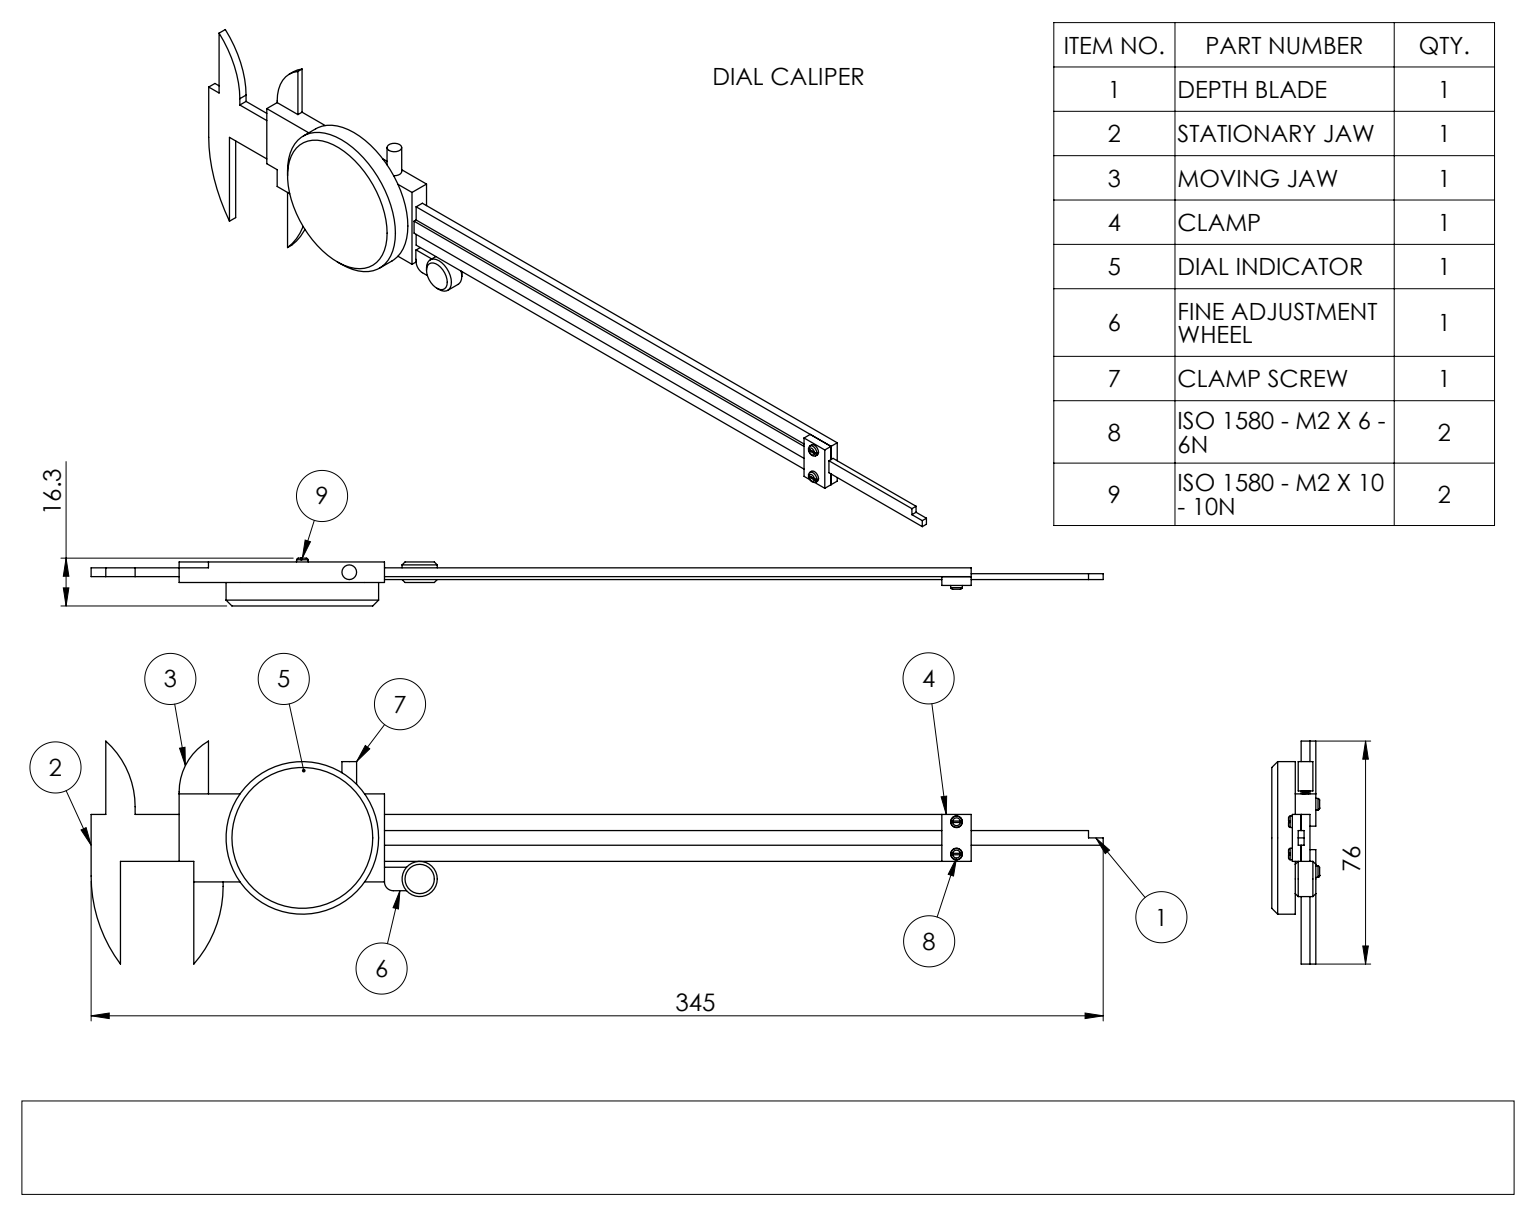
ISO-10303-21;
HEADER;
FILE_DESCRIPTION (('STEP AP214'),
    '1' );
FILE_NAME ('MAS-164',
    '2026-10-27T04:40:18',
    ( '' ),
    ( '' ),
    'SwSTEP 2.0',
    'SolidWorks 2026',
    '' );
FILE_SCHEMA (( 'AUTOMOTIVE_DESIGN' ));
ENDSEC;

DATA;
#1 = CARTESIAN_POINT ( 'NONE',  ( -49.99998799999998766, -10.00000000000001066, -0.1418111474832477736 ) ) ;
#2 = CARTESIAN_POINT ( 'NONE',  ( -60.99999999999998579, 10.72916666666666607, 2.077350269189628840 ) ) ;
#3 = CARTESIAN_POINT ( 'NONE',  ( -62.86468353124999453, 12.51562499965860198, 1.500000000000002220 ) ) ;
#4 = CARTESIAN_POINT ( 'NONE',  ( -62.43234176562498305, 9.411458332991935904, 0.7511620957034662593 ) ) ;
#5 = DIRECTION ( 'NONE',  ( 0.000000000000000000, 0.000000000000000000, -1.000000000000000000 ) ) ;
#6 = ADVANCED_FACE ( 'NONE', ( #7611 ), #3122, .F. ) ;
#7 = CARTESIAN_POINT ( 'NONE',  ( -61.99999999999998579, 16.00000000000000000, 1.500000000000002220 ) ) ;
#8 = CARTESIAN_POINT ( 'NONE',  ( -62.43234176562498305, 9.223958332991935904, 0.7511620957034662593 ) ) ;
#9 = CARTESIAN_POINT ( 'NONE',  ( 0.5000000000000000000, 0.2499999999999982792, -1.911797424705720339 ) ) ;
#10 = ORIENTED_EDGE ( 'NONE', *, *, #8889, .F. ) ;
#11 = FACE_OUTER_BOUND ( 'NONE', #2535, .T. ) ;
#12 = DIRECTION ( 'NONE',  ( -1.000000000000000000, 0.000000000000000000, 0.000000000000000000 ) ) ;
#13 = ADVANCED_FACE ( 'NONE', ( #1458 ), #5708, .T. ) ;
#14 = CARTESIAN_POINT ( 'NONE',  ( -62.86468353124998032, 15.68229166632526628, 1.000774730468978024 ) ) ;
#15 = CARTESIAN_POINT ( 'NONE',  ( -61.99999999999998579, 11.14062499965860020, 0.5015494609379544944 ) ) ;
#16 = CARTESIAN_POINT ( 'NONE',  ( -62.86468353124999453, 16.03645833299193768, 1.999225269531025750 ) ) ;
#17 = CARTESIAN_POINT ( 'NONE',  ( -61.49999999999998579, 9.677083332650534331, 2.366025403784441927 ) ) ;
#18 = ORIENTED_EDGE ( 'NONE', *, *, #1732, .F. ) ;
#19 = CARTESIAN_POINT ( 'NONE',  ( -62.49999999999998579, 14.58333333333333393, 0.6339745962155627357 ) ) ;
#20 = ADVANCED_FACE ( 'NONE', ( #3172 ), #5726, .T. ) ;
#21 = CARTESIAN_POINT ( 'NONE',  ( -61.56765823437498852, 8.598958332991934128, 2.248837904296538515 ) ) ;
#22 = SHAPE_REPRESENTATION_RELATIONSHIP ( 'NONE' , 'NONE' ,  #8867, #2558 ) ;
#23 = CARTESIAN_POINT ( 'NONE',  ( -61.49999999999998579, 13.67708333265053433, 2.366025403784441927 ) ) ;
#24 = VERTEX_POINT ( 'NONE', #10006 ) ;
#25 = DIRECTION ( 'NONE',  ( -1.000000000000000000, -0.000000000000000000, -0.000000000000000000 ) ) ;
#26 =( BOUNDED_CURVE ( )  B_SPLINE_CURVE ( 2, ( #4662, #10727, #5554, #5432, #3111, #6399, #1393, #5495, #3837 ),
 .UNSPECIFIED., .F., .T. ) 
 B_SPLINE_CURVE_WITH_KNOTS ( ( 3, 2, 2, 2, 3 ),
 ( 0.3984375000000000000, 0.4010416666666666852, 0.4062500000000000000, 0.4114583333333333148, 0.4140625000000000000 ),
 .UNSPECIFIED. ) 
 CURVE ( )  GEOMETRIC_REPRESENTATION_ITEM ( )  RATIONAL_B_SPLINE_CURVE ( ( 0.9330127018922194093, 0.9330127018922194093, 1.000000000000000000, 0.8660254037844387076, 1.000000000000000000, 0.8660254037844387076, 1.000000000000000000, 0.9330127018922194093, 0.9330127018922194093 ) ) 
 REPRESENTATION_ITEM ( '' )  );
#27 = CARTESIAN_POINT ( 'NONE',  ( -62.86468353124998032, 11.68229166632526983, 1.000774730468978024 ) ) ;
#28 = DIRECTION ( 'NONE',  ( -1.000000000000000000, 0.000000000000000000, 0.000000000000000000 ) ) ;
#29 = ORIENTED_EDGE ( 'NONE', *, *, #855, .F. ) ;
#30 = LINE ( 'NONE', #3412, #7519 ) ;
#31 = CARTESIAN_POINT ( 'NONE',  ( -62.86468353124998742, 13.28645833299193413, 1.999225269531025972 ) ) ;
#32 = CARTESIAN_POINT ( 'NONE',  ( -61.99999999999998579, 11.65624999931720218, 2.500000000000002665 ) ) ;
#33 = ORIENTED_EDGE ( 'NONE', *, *, #3045, .T. ) ;
#34 = CARTESIAN_POINT ( 'NONE',  ( -149.9999999999999716, 8.000000000000000000, 0.000000000000000000 ) ) ;
#35 = VERTEX_POINT ( 'NONE', #9289 ) ;
#36 = DIRECTION ( 'NONE',  ( 1.000000000000000000, 0.000000000000000000, 0.000000000000000000 ) ) ;
#37 = AXIS2_PLACEMENT_3D ( 'NONE', #4538, #3831, #10428 ) ;
#38 = AXIS2_PLACEMENT_3D ( 'NONE', #7635, #10225, #6696 ) ;
#39 = ADVANCED_FACE ( 'NONE', ( #10062, #3972, #586 ), #1625, .F. ) ;
#40 = VERTEX_POINT ( 'NONE', #7517 ) ;
#41 = VERTEX_POINT ( 'NONE', #5843 ) ;
#42 = CARTESIAN_POINT ( 'NONE',  ( -61.99999999999998579, 8.703124999658601979, 0.5015494609379544944 ) ) ;
#43 = CARTESIAN_POINT ( 'NONE',  ( -61.99999999999998579, 15.93749999999999645, 2.500000000000002665 ) ) ;
#44 = AXIS2_PLACEMENT_3D ( 'NONE', #893, #1059, #6847 ) ;
#45 = CARTESIAN_POINT ( 'NONE',  ( -61.13531646874998415, 12.66145833299193413, 1.000774730468978468 ) ) ;
#46 = ORIENTED_EDGE ( 'NONE', *, *, #9999, .T. ) ;
#47 = DIRECTION ( 'NONE',  ( -0.000000000000000000, -0.000000000000000000, -1.000000000000000000 ) ) ;
#48 = PRODUCT ( 'moving jaw', 'moving jaw', '', ( #5785 ) ) ;
#49 = EDGE_LOOP ( 'NONE', ( #4259, #9067, #9089, #3500, #4349, #3630, #6139, #9782 ) ) ;
#50 = AXIS2_PLACEMENT_3D ( 'NONE', #1912, #8752, #7861 ) ;
#51 = CARTESIAN_POINT ( 'NONE',  ( -62.99999999999998579, 11.57291666598387003, 0.9226497308103756012 ) ) ;
#52 = CARTESIAN_POINT ( 'NONE',  ( -62.43234176562498305, 15.66145833299193590, 0.7511620957034662593 ) ) ;
#53 = CARTESIAN_POINT ( 'NONE',  ( 144.0000000000000284, -5.500000000000000000, 3.000000000000000000 ) ) ;
#54 = CARTESIAN_POINT ( 'NONE',  ( -61.49999999999998579, 12.51041666598386826, 0.6339745962155628467 ) ) ;
#55 = CARTESIAN_POINT ( 'NONE',  ( -62.99999999999998579, 8.854166666666666075, 0.9226497308103756012 ) ) ;
#56 = CARTESIAN_POINT ( 'NONE',  ( -61.13531646874997705, 12.41145833299193413, 1.000774730468978468 ) ) ;
#57 = EDGE_CURVE ( 'NONE', #2237, #10334, #9260, .T. ) ;
#58 = CARTESIAN_POINT ( 'NONE',  ( -61.13531646874998415, 9.057291666325266277, 1.999225269531026417 ) ) ;
#59 = CARTESIAN_POINT ( 'NONE',  ( -61.49999999999998579, 9.208333333333333925, 2.366025403784441927 ) ) ;
#60 = DIRECTION ( 'NONE',  ( -1.000000000000000000, -0.000000000000000000, -0.000000000000000000 ) ) ;
#61 = CARTESIAN_POINT ( 'NONE',  ( -61.13531646874998415, 9.661458332991932352, 1.000774730468978468 ) ) ;
#62 = CARTESIAN_POINT ( 'NONE',  ( -62.99999999999998579, 14.07291666598387003, 0.9226497308103756012 ) ) ;
#63 = ORIENTED_EDGE ( 'NONE', *, *, #6322, .T. ) ;
#64 = VECTOR ( 'NONE', #9723, 1000.000000000000000 ) ;
#65 = CARTESIAN_POINT ( 'NONE',  ( -61.99999999999998579, 12.81250000000000000, 0.5000000000000013323 ) ) ;
#66 = CARTESIAN_POINT ( 'NONE',  ( -61.73205080756886076, 11.16741454900183328, 2.500000000000003109 ) ) ;
#67 = CARTESIAN_POINT ( 'NONE',  ( -61.99999999999999289, 15.14062499965860198, 0.5015494609379544944 ) ) ;
#68 = CARTESIAN_POINT ( 'NONE',  ( -62.43234176562499016, 10.74479166632526805, 2.248837904296538071 ) ) ;
#69 = CARTESIAN_POINT ( 'NONE',  ( -61.99999999999999289, 15.82812499965860198, 2.498450539062049724 ) ) ;
#70 = CARTESIAN_POINT ( 'NONE',  ( -37.99999999999999289, -14.00000000000000888, -2.000000000000000000 ) ) ;
#71 = EDGE_LOOP ( 'NONE', ( #7087, #10551, #5486, #977 ) ) ;
#72 = CARTESIAN_POINT ( 'NONE',  ( -62.49999999999998579, 15.08333333333333393, 0.6339745962155627357 ) ) ;
#73 = CARTESIAN_POINT ( 'NONE',  ( -62.86468353124999453, 8.286458332991934128, 1.999225269531025750 ) ) ;
#74 = CARTESIAN_POINT ( 'NONE',  ( -62.49999999999998579, 13.30208333265053433, 0.6339745962155627357 ) ) ;
#75 = CARTESIAN_POINT ( 'NONE',  ( -62.99999999999998579, 13.12500000000000178, 1.500000000000001998 ) ) ;
#76 = CARTESIAN_POINT ( 'NONE',  ( -61.99999999999998579, 9.812500000000000000, 0.5000000000000013323 ) ) ;
#77 = CARTESIAN_POINT ( 'NONE',  ( -61.56765823437498852, 11.03645833299193590, 2.248837904296538515 ) ) ;
#78 =( NAMED_UNIT ( * ) SI_UNIT ( $, .STERADIAN. ) SOLID_ANGLE_UNIT ( ) );
#79 = CARTESIAN_POINT ( 'NONE',  ( -61.99999999999997868, 8.312499999999998224, 0.5000000000000013323 ) ) ;
#80 = ORIENTED_EDGE ( 'NONE', *, *, #3705, .F. ) ;
#81 = CARTESIAN_POINT ( 'NONE',  ( -61.99999999999998579, 12.15624999931720041, 2.500000000000002665 ) ) ;
#82 = CARTESIAN_POINT ( 'NONE',  ( -61.13531646874998415, 13.16145833299193413, 1.000774730468978468 ) ) ;
#83 = SHAPE_REPRESENTATION_RELATIONSHIP ( 'NONE' , 'NONE' ,  #2047, #5753 ) ;
#84 = DIRECTION ( 'NONE',  ( -0.000000000000000000, -1.000000000000000000, -0.000000000000000000 ) ) ;
#85 = CARTESIAN_POINT ( 'NONE',  ( -60.99999999999998579, 8.697916665983868256, 2.077350269189628840 ) ) ;
#86 = ORIENTED_EDGE ( 'NONE', *, *, #4258, .T. ) ;
#87 =( BOUNDED_CURVE ( )  B_SPLINE_CURVE ( 2, ( #8357, #10903, #5902, #8456, #10798, #841, #3187, #174, #6119 ),
 .UNSPECIFIED., .F., .T. ) 
 B_SPLINE_CURVE_WITH_KNOTS ( ( 3, 2, 2, 2, 3 ),
 ( 0.5703125000000000000, 0.5729166666666666297, 0.5781250000000000000, 0.5833333333333333703, 0.5859375000000000000 ),
 .UNSPECIFIED. ) 
 CURVE ( )  GEOMETRIC_REPRESENTATION_ITEM ( )  RATIONAL_B_SPLINE_CURVE ( ( 0.9330127018922194093, 0.9330127018922194093, 1.000000000000000000, 0.8660254037844387076, 1.000000000000000000, 0.8660254037844387076, 1.000000000000000000, 0.9330127018922194093, 0.9330127018922194093 ) ) 
 REPRESENTATION_ITEM ( '' )  );
#88 = DIRECTION ( 'NONE',  ( -0.000000000000000000, 1.000000000000000000, 1.224646799147353207E-16 ) ) ;
#89 = ORIENTED_EDGE ( 'NONE', *, *, #6443, .F. ) ;
#90 = CARTESIAN_POINT ( 'NONE',  ( 11.30000000000000426, 1.224646799147353207E-16, -1.000000000000000000 ) ) ;
#91 = EDGE_CURVE ( 'NONE', #7478, #353, #1465, .T. ) ;
#92 = CARTESIAN_POINT ( 'NONE',  ( -62.43234176562498305, 11.91145833299193413, 0.7511620957034662593 ) ) ;
#93 = ORIENTED_EDGE ( 'NONE', *, *, #6556, .F. ) ;
#94 = CARTESIAN_POINT ( 'NONE',  ( -62.43234176562499016, 9.057291666325268054, 2.248837904296538071 ) ) ;
#95 = LINE ( 'NONE', #7549, #8153 ) ;
#96 = CARTESIAN_POINT ( 'NONE',  ( -61.56765823437498852, 12.59895833299193413, 2.248837904296538515 ) ) ;
#97 = EDGE_CURVE ( 'NONE', #8537, #7681, #4845, .T. ) ;
#98 = CARTESIAN_POINT ( 'NONE',  ( -61.99999999999998579, 8.281249999317202182, 0.5000000000000013323 ) ) ;
#99 = ORIENTED_EDGE ( 'NONE', *, *, #1134, .T. ) ;
#100 = CARTESIAN_POINT ( 'NONE',  ( -61.99999999999998579, 16.00000000000000000, 2.500000000000000444 ) ) ;
#101 = ORIENTED_EDGE ( 'NONE', *, *, #9521, .F. ) ;
#102 = CARTESIAN_POINT ( 'NONE',  ( -61.73205080756886076, 14.27008544963257108, 0.5000000000000014433 ) ) ;
#103 = CARTESIAN_POINT ( 'NONE',  ( -61.13531646874998415, 15.30729166632526983, 1.999225269531026417 ) ) ;
#104 = FACE_OUTER_BOUND ( 'NONE', #8107, .T. ) ;
#105 = CARTESIAN_POINT ( 'NONE',  ( 140.0000000000000284, 8.000000000000000000, 3.000000000000000000 ) ) ;
#106 = CARTESIAN_POINT ( 'NONE',  ( -62.49999999999998579, 12.30208333265053611, 0.6339745962155627357 ) ) ;
#107 = EDGE_CURVE ( 'NONE', #8110, #4251, #4105, .T. ) ;
#108 = CARTESIAN_POINT ( 'NONE',  ( -61.56765823437498852, 14.34895833299193413, 2.248837904296538515 ) ) ;
#109 = CARTESIAN_POINT ( 'NONE',  ( -62.43234176562499016, 8.494791666325268054, 2.248837904296538071 ) ) ;
#110 = CARTESIAN_POINT ( 'NONE',  ( -61.99999999999998579, 9.187500000000000000, 2.500000000000002665 ) ) ;
#111 = LINE ( 'NONE', #735, #8321 ) ;
#112 = CARTESIAN_POINT ( 'NONE',  ( -61.56765823437498142, 8.682291666325268054, 0.7511620957034663704 ) ) ;
#113 = ADVANCED_FACE ( 'NONE', ( #788 ), #9184, .T. ) ;
#114 = CARTESIAN_POINT ( 'NONE',  ( -62.49999999999998579, 14.05208333265053611, 0.6339745962155627357 ) ) ;
#115 = EDGE_LOOP ( 'NONE', ( #2530, #9133, #537, #4365 ) ) ;
#116 = PLANE ( 'NONE',  #5116 ) ;
#117 = DIRECTION ( 'NONE',  ( 0.000000000000000000, 0.000000000000000000, 1.000000000000000000 ) ) ;
#118 = EDGE_CURVE ( 'NONE', #7049, #4198, #6685, .T. ) ;
#119 = CARTESIAN_POINT ( 'NONE',  ( -61.13531646874998415, 15.07812499965860020, 1.500000000000002220 ) ) ;
#120 = CARTESIAN_POINT ( 'NONE',  ( -62.86468353124998032, 10.93229166632526805, 1.000774730468978246 ) ) ;
#121 = CARTESIAN_POINT ( 'NONE',  ( -61.56765823437498852, 9.536458332991934128, 2.248837904296538515 ) ) ;
#122 = ORIENTED_EDGE ( 'NONE', *, *, #10904, .T. ) ;
#123 = CARTESIAN_POINT ( 'NONE',  ( -62.99999999999998579, 15.12500000000000000, 1.500000000000001998 ) ) ;
#124 = CARTESIAN_POINT ( 'NONE',  ( -61.13531646874998415, 9.640624999658601979, 1.500000000000002220 ) ) ;
#125 = AXIS2_PLACEMENT_3D ( 'NONE', #8648, #2761, #6933 ) ;
#126 = CARTESIAN_POINT ( 'NONE',  ( 0.000000000000000000, 0.000000000000000000, 0.000000000000000000 ) ) ;
#127 = CARTESIAN_POINT ( 'NONE',  ( -61.49999999999998579, 13.76041666598387003, 0.6339745962155628467 ) ) ;
#128 = ORIENTED_EDGE ( 'NONE', *, *, #1993, .F. ) ;
#129 = CARTESIAN_POINT ( 'NONE',  ( -61.99999999999998579, 14.90624999931720218, 2.500000000000002665 ) ) ;
#130 = VECTOR ( 'NONE', #9095, 1000.000000000000000 ) ;
#131 = CARTESIAN_POINT ( 'NONE',  ( -62.86468353124999453, 11.97395833299193413, 1.999225269531025750 ) ) ;
#132 =( NAMED_UNIT ( * ) PLANE_ANGLE_UNIT ( ) SI_UNIT ( $, .RADIAN. ) );
#133 = LINE ( 'NONE', #9524, #10148 ) ;
#134 = ORIENTED_EDGE ( 'NONE', *, *, #6586, .T. ) ;
#135 = CARTESIAN_POINT ( 'NONE',  ( -105.0000000000000000, 2.500000000000000000, 4.000000000000000000 ) ) ;
#136 = CARTESIAN_POINT ( 'NONE',  ( -61.13531646874998415, 12.91145833299193590, 1.000774730468978468 ) ) ;
#137 = FILL_AREA_STYLE ('',( #1868 ) ) ;
#138 = CARTESIAN_POINT ( 'NONE',  ( -60.99999999999998579, 10.22916666666666785, 2.077350269189628840 ) ) ;
#139 = VECTOR ( 'NONE', #2970, 1000.000000000000000 ) ;
#140 = CARTESIAN_POINT ( 'NONE',  ( -62.49999999999998579, 9.302083332650536107, 0.6339745962155627357 ) ) ;
#141 = EDGE_CURVE ( 'NONE', #5618, #1714, #3939, .T. ) ;
#142 = ORIENTED_EDGE ( 'NONE', *, *, #7024, .F. ) ;
#143 = CARTESIAN_POINT ( 'NONE',  ( -61.73205080756886076, 14.05133545031537068, 0.5000000000000014433 ) ) ;
#144 = CIRCLE ( 'NONE', #2107, 1.000000000000000888 ) ;
#145 = CARTESIAN_POINT ( 'NONE',  ( -62.26794919243111082, 15.29241454900183328, 0.5000000000000013323 ) ) ;
#146 = EDGE_CURVE ( 'NONE', #6970, #9736, #4895, .T. ) ;
#147 = CARTESIAN_POINT ( 'NONE',  ( -61.13531646874998415, 11.05729166632526805, 1.999225269531026417 ) ) ;
#148 = VECTOR ( 'NONE', #1244, 1000.000000000000000 ) ;
#149 = ORIENTED_EDGE ( 'NONE', *, *, #772, .F. ) ;
#150 = VECTOR ( 'NONE', #8789, 1000.000000000000000 ) ;
#151 = CARTESIAN_POINT ( 'NONE',  ( -61.13531646874998415, 8.411458332991934128, 1.000774730468978468 ) ) ;
#152 = PLANE ( 'NONE',  #5103 ) ;
#153 = EDGE_CURVE ( 'NONE', #9355, #9315, #9914, .T. ) ;
#154 = VECTOR ( 'NONE', #5685, 1000.000000000000000 ) ;
#155 = CARTESIAN_POINT ( 'NONE',  ( -61.56765823437498852, 14.09895833299193413, 2.248837904296538515 ) ) ;
#156 = CARTESIAN_POINT ( 'NONE',  ( -62.49999999999998579, 9.302083332650536107, 0.6339745962155627357 ) ) ;
#157 = ORIENTED_EDGE ( 'NONE', *, *, #473, .F. ) ;
#158 = FACE_OUTER_BOUND ( 'NONE', #3006, .T. ) ;
#159 = ORIENTED_EDGE ( 'NONE', *, *, #10440, .T. ) ;
#160 = CARTESIAN_POINT ( 'NONE',  ( -62.49999999999998579, 10.83333333333333393, 0.6339745962155627357 ) ) ;
#161 = CARTESIAN_POINT ( 'NONE',  ( -62.99999999999998579, 8.104166666666667851, 0.9226497308103756012 ) ) ;
#162 = AXIS2_PLACEMENT_3D ( 'NONE', #9186, #3975, #9242 ) ;
#163 = CARTESIAN_POINT ( 'NONE',  ( -61.99999999999997868, 8.781249999317202182, 0.5000000000000013323 ) ) ;
#164 = DIRECTION ( 'NONE',  ( -0.000000000000000000, -1.000000000000000000, -0.000000000000000000 ) ) ;
#165 = CARTESIAN_POINT ( 'NONE',  ( -61.73205080756888208, 10.69866454968463110, 2.500000000000006661 ) ) ;
#166 = CARTESIAN_POINT ( 'NONE',  ( -61.13531646874997705, 13.41145833299193413, 1.000774730468978468 ) ) ;
#167 = CARTESIAN_POINT ( 'NONE',  ( -61.56765823437498142, 8.869791666325268054, 0.7511620957034663704 ) ) ;
#168 = LINE ( 'NONE', #6113, #341 ) ;
#169 = PLANE ( 'NONE',  #3525 ) ;
#170 = CARTESIAN_POINT ( 'NONE',  ( -62.86468353124998742, 9.786458332991934128, 1.999225269531025972 ) ) ;
#171 = CARTESIAN_POINT ( 'NONE',  ( -77.99999999999998579, 11.49999999999999645, 4.999999999999999112 ) ) ;
#172 = ORIENTED_EDGE ( 'NONE', *, *, #7897, .T. ) ;
#173 = DIRECTION ( 'NONE',  ( -0.000000000000000000, -0.000000000000000000, 1.000000000000000000 ) ) ;
#174 = CARTESIAN_POINT ( 'NONE',  ( -62.26794919243111082, 12.67633545031537068, 2.500000000000003109 ) ) ;
#175 = EDGE_CURVE ( 'NONE', #2979, #4700, #8697, .T. ) ;
#176 = PRODUCT_DEFINITION_FORMATION_WITH_SPECIFIED_SOURCE ( 'ANY', '', #2270, .NOT_KNOWN. ) ;
#177 = CARTESIAN_POINT ( 'NONE',  ( -62.43234176562499016, 14.99479166632526805, 2.248837904296538071 ) ) ;
#178 = CARTESIAN_POINT ( 'NONE',  ( -62.86468353124998742, 11.47395833299193590, 1.999225269531025972 ) ) ;
#179 = ADVANCED_BREP_SHAPE_REPRESENTATION ( '', ( #4912, #2307 ), #5679 ) ;
#180 = ADVANCED_FACE ( 'NONE', ( #9080 ), #7568, .T. ) ;
#181 = CARTESIAN_POINT ( 'NONE',  ( -61.13531646874998415, 8.578124999658601979, 1.500000000000002220 ) ) ;
#182 = CARTESIAN_POINT ( 'NONE',  ( -61.99999999999998579, 11.40624999931720218, 2.500000000000002665 ) ) ;
#183 = ORIENTED_EDGE ( 'NONE', *, *, #3221, .T. ) ;
#184 = CARTESIAN_POINT ( 'NONE',  ( -62.99999999999998579, 14.60416666666666785, 0.9226497308103756012 ) ) ;
#185 = CARTESIAN_POINT ( 'NONE',  ( -61.56765823437498852, 10.09895833299193413, 2.248837904296538515 ) ) ;
#186 = CARTESIAN_POINT ( 'NONE',  ( -62.99999999999998579, 13.59374999931720218, 1.500000000000001998 ) ) ;
#187 = CARTESIAN_POINT ( 'NONE',  ( -120.0000000000000000, -4.000000000000019540, -2.000000000000000000 ) ) ;
#188 = ORIENTED_EDGE ( 'NONE', *, *, #5061, .T. ) ;
#189 = CYLINDRICAL_SURFACE ( 'NONE', #9638, 0.9999999999999981126 ) ;
#190 = CARTESIAN_POINT ( 'NONE',  ( -62.86468353124998032, 10.93229166632526805, 1.000774730468978024 ) ) ;
#191 = CARTESIAN_POINT ( 'NONE',  ( -60.99999999999998579, 13.00000000000000178, 1.500000000000002220 ) ) ;
#192 = VERTEX_POINT ( 'NONE', #7412 ) ;
#193 = CARTESIAN_POINT ( 'NONE',  ( -62.49999999999998579, 10.58333333333333393, 0.6339745962155627357 ) ) ;
#194 = CARTESIAN_POINT ( 'NONE',  ( -61.73205080756886076, 15.91741454900183150, 2.500000000000003109 ) ) ;
#195 = CARTESIAN_POINT ( 'NONE',  ( -62.86468353124999453, 14.26562499965860020, 1.500000000000002220 ) ) ;
#196 = CARTESIAN_POINT ( 'NONE',  ( -62.49999999999998579, 13.91666666666666785, 2.366025403784441483 ) ) ;
#197 = ADVANCED_FACE ( 'NONE', ( #5899 ), #8198, .T. ) ;
#198 = CARTESIAN_POINT ( 'NONE',  ( -62.99999999999998579, 8.614583332650536107, 2.077350269189627952 ) ) ;
#199 = EDGE_LOOP ( 'NONE', ( #1282, #1739, #251, #2267 ) ) ;
#200 = AXIS2_PLACEMENT_3D ( 'NONE', #7285, #4873, #3159 ) ;
#201 = LINE ( 'NONE', #377, #2655 ) ;
#202 = CARTESIAN_POINT ( 'NONE',  ( -61.73205080756886076, 10.02008544963257464, 0.5000000000000014433 ) ) ;
#203 = CARTESIAN_POINT ( 'NONE',  ( -61.56765823437498142, 11.36979166632526805, 0.7511620957034663704 ) ) ;
#204 =( NAMED_UNIT ( * ) PLANE_ANGLE_UNIT ( ) SI_UNIT ( $, .RADIAN. ) );
#205 = ORIENTED_EDGE ( 'NONE', *, *, #5925, .T. ) ;
#206 = CLOSED_SHELL ( 'NONE', ( #8673, #5883, #7933, #4871, #589, #6929, #9618, #1051, #39, #10363, #9693, #7084, #2486, #5406 ) ) ;
#207 = CARTESIAN_POINT ( 'NONE',  ( -61.13531646874998415, 10.91145833299193590, 1.000774730468978468 ) ) ;
#208 = LINE ( 'NONE', #3594, #2451 ) ;
#209 = CARTESIAN_POINT ( 'NONE',  ( -61.13531646874998415, 14.16145833299193413, 1.000774730468978468 ) ) ;
#210 = CARTESIAN_POINT ( 'NONE',  ( -62.26794919243111082, 9.292414549001833279, 0.5000000000000013323 ) ) ;
#211 = VERTEX_POINT ( 'NONE', #6639 ) ;
#212 = AXIS2_PLACEMENT_3D ( 'NONE', #5369, #8063, #3772 ) ;
#213 = CARTESIAN_POINT ( 'NONE',  ( 0.5000000000000000000, -0.2499999999999997780, -1.911797424705720116 ) ) ;
#214 = VECTOR ( 'NONE', #3123, 1000.000000000000000 ) ;
#215 = B_SPLINE_CURVE_WITH_KNOTS ( 'NONE', 3,
 ( #10711, #8988, #7212, #4753, #3985, #5646 ),
 .UNSPECIFIED., .F., .F.,
 ( 4, 2, 4 ),
 ( 0.0005861251363949651497, 0.001008091297609326311, 0.001430057458823687363 ),
 .UNSPECIFIED. ) ;
#216 = ORIENTED_EDGE ( 'NONE', *, *, #8132, .T. ) ;
#217 = CARTESIAN_POINT ( 'NONE',  ( -61.99999999999998579, 15.03124999931720218, 0.5000000000000013323 ) ) ;
#218 = CARTESIAN_POINT ( 'NONE',  ( -61.99999999999998579, 8.437500000000000000, 2.654700538379254571 ) ) ;
#219 = CARTESIAN_POINT ( 'NONE',  ( -61.99999999999998579, 13.68749999999999822, 2.500000000000002665 ) ) ;
#220 = DIRECTION ( 'NONE',  ( -1.000000000000000000, -3.469446951953572774E-16, 0.000000000000000000 ) ) ;
#221 = DIRECTION ( 'NONE',  ( -0.000000000000000000, -1.000000000000000000, -0.000000000000000000 ) ) ;
#222 = AXIS2_PLACEMENT_3D ( 'NONE', #2692, #4339, #10352 ) ;
#223 = CARTESIAN_POINT ( 'NONE',  ( -62.86468353124998032, 14.49479166632526983, 1.000774730468978024 ) ) ;
#224 = VECTOR ( 'NONE', #3060, 999.9999999999998863 ) ;
#225 = CARTESIAN_POINT ( 'NONE',  ( -61.99999999999998579, 8.515624999658601979, 2.498450539062049724 ) ) ;
#226 = CARTESIAN_POINT ( 'NONE',  ( -62.99999999999998579, 11.32291666598387181, 0.9226497308103756012 ) ) ;
#227 = FACE_OUTER_BOUND ( 'NONE', #9637, .T. ) ;
#228 = CARTESIAN_POINT ( 'NONE',  ( -61.13531646874998415, 10.11979166632526805, 1.999225269531026417 ) ) ;
#229 = CARTESIAN_POINT ( 'NONE',  ( -61.99999999999998579, 14.03124999931720218, 0.5000000000000013323 ) ) ;
#230 = ORIENTED_EDGE ( 'NONE', *, *, #4677, .T. ) ;
#231 = DIRECTION ( 'NONE',  ( -1.000000000000000000, 0.000000000000000000, 0.000000000000000000 ) ) ;
#232 = CARTESIAN_POINT ( 'NONE',  ( -61.99999999999998579, 13.03124999931720218, 0.5000000000000013323 ) ) ;
#233 = APPLICATION_CONTEXT ( 'automotive_design' ) ;
#234 = VECTOR ( 'NONE', #2072, 1000.000000000000000 ) ;
#235 = CARTESIAN_POINT ( 'NONE',  ( -61.13531646874997705, 15.59895833299193590, 1.000774730468978468 ) ) ;
#236 = CARTESIAN_POINT ( 'NONE',  ( -61.56765823437498852, 13.03645833299193413, 2.248837904296538515 ) ) ;
#237 = CARTESIAN_POINT ( 'NONE',  ( -61.99999999999999289, 8.265624999658601979, 2.498450539062049724 ) ) ;
#238 = ORIENTED_EDGE ( 'NONE', *, *, #10620, .F. ) ;
#239 = CARTESIAN_POINT ( 'NONE',  ( -62.26794919243111082, 14.07366454968463110, 0.5000000000000013323 ) ) ;
#240 = CARTESIAN_POINT ( 'NONE',  ( -62.43234176562499016, 9.557291666325268054, 2.248837904296538071 ) ) ;
#241 = CARTESIAN_POINT ( 'NONE',  ( -61.56765823437498852, 14.78645833299193413, 2.248837904296538515 ) ) ;
#242 = AXIS2_PLACEMENT_3D ( 'NONE', #968, #2330, #9109 ) ;
#243 = CARTESIAN_POINT ( 'NONE',  ( -61.99999999999998579, 14.28124999931720396, 0.3452994616207497591 ) ) ;
#244 = LINE ( 'NONE', #5283, #6807 ) ;
#245 = ORIENTED_EDGE ( 'NONE', *, *, #9568, .F. ) ;
#246 = CARTESIAN_POINT ( 'NONE',  ( -61.73205080756886076, 9.801335450315370679, 0.5000000000000014433 ) ) ;
#247 = ADVANCED_FACE ( 'NONE', ( #10016 ), #2398, .F. ) ;
#248 = CARTESIAN_POINT ( 'NONE',  ( -61.13531646874998415, 12.07812499965860198, 1.500000000000002220 ) ) ;
#249 = CYLINDRICAL_SURFACE ( 'NONE', #10424, 0.9999999999999981126 ) ;
#250 = DIRECTION ( 'NONE',  ( 1.000000000000000000, 0.000000000000000000, 0.000000000000000000 ) ) ;
#251 = ORIENTED_EDGE ( 'NONE', *, *, #8511, .F. ) ;
#252 = CARTESIAN_POINT ( 'NONE',  ( -61.49999999999998579, 11.04166666666666607, 0.6339745962155628467 ) ) ;
#253 = CARTESIAN_POINT ( 'NONE',  ( -61.99999999999998579, 8.531249999317203958, 0.5000000000000013323 ) ) ;
#254 = CARTESIAN_POINT ( 'NONE',  ( -61.99999999999998579, 14.57812499965860198, 2.498450539062049724 ) ) ;
#255 =( BOUNDED_CURVE ( )  B_SPLINE_CURVE ( 2, ( #5430, #6282, #8897, #2058, #9721, #9666, #6225, #10606, #9607 ),
 .UNSPECIFIED., .F., .T. ) 
 B_SPLINE_CURVE_WITH_KNOTS ( ( 3, 2, 2, 2, 3 ),
 ( 0.08593750000000000000, 0.08854166666666667129, 0.09375000000000000000, 0.09895833333333332871, 0.1015625000000000833 ),
 .UNSPECIFIED. ) 
 CURVE ( )  GEOMETRIC_REPRESENTATION_ITEM ( )  RATIONAL_B_SPLINE_CURVE ( ( 0.9330127018922194093, 0.9330127018922194093, 1.000000000000000000, 0.8660254037844387076, 1.000000000000000000, 0.8660254037844387076, 1.000000000000000000, 0.9330127018922171889, 0.9330127018922194093 ) ) 
 REPRESENTATION_ITEM ( '' )  );
#256 =( NAMED_UNIT ( * ) SI_UNIT ( $, .STERADIAN. ) SOLID_ANGLE_UNIT ( ) );
#257 = CARTESIAN_POINT ( 'NONE',  ( -61.99999999999998579, 13.93749999999999822, 2.500000000000002665 ) ) ;
#258 = CARTESIAN_POINT ( 'NONE',  ( -62.99999999999998579, 9.364583332650536107, 2.077350269189627952 ) ) ;
#259 = ORIENTED_EDGE ( 'NONE', *, *, #9835, .T. ) ;
#260 = CARTESIAN_POINT ( 'NONE',  ( -61.49999999999998579, 13.54166666666666785, 0.6339745962155628467 ) ) ;
#261 = CARTESIAN_POINT ( 'NONE',  ( -62.49999999999998579, 15.38541666598387003, 2.366025403784441483 ) ) ;
#262 = CARTESIAN_POINT ( 'NONE',  ( -62.43234176562499016, 10.74479166632526805, 2.248837904296538071 ) ) ;
#263 = ADVANCED_FACE ( 'NONE', ( #7011 ), #2615, .T. ) ;
#264 = ORIENTED_EDGE ( 'NONE', *, *, #1352, .F. ) ;
#265 = CARTESIAN_POINT ( 'NONE',  ( -62.43234176562499016, 10.05729166632526805, 2.248837904296538071 ) ) ;
#266 = DIRECTION ( 'NONE',  ( -0.000000000000000000, -0.000000000000000000, -1.000000000000000000 ) ) ;
#267 = CARTESIAN_POINT ( 'NONE',  ( -61.13531646874998415, 13.86979166632526805, 1.999225269531026417 ) ) ;
#268 = DIRECTION ( 'NONE',  ( -1.000000000000000000, 0.000000000000000000, 0.000000000000000000 ) ) ;
#269 = ORIENTED_EDGE ( 'NONE', *, *, #9235, .F. ) ;
#270 = CARTESIAN_POINT ( 'NONE',  ( 0.000000000000000000, -0.2499999999999998335, -1.312875263449798879 ) ) ;
#271 = ORIENTED_EDGE ( 'NONE', *, *, #9771, .F. ) ;
#272 = DIRECTION ( 'NONE',  ( 0.000000000000000000, 0.000000000000000000, -1.000000000000000000 ) ) ;
#273 = CARTESIAN_POINT ( 'NONE',  ( -62.49999999999998579, 8.416666666666666075, 2.366025403784441483 ) ) ;
#274 = LINE ( 'NONE', #989, #4138 ) ;
#275 = DIRECTION ( 'NONE',  ( -0.000000000000000000, -1.000000000000000000, -0.000000000000000000 ) ) ;
#276 = DIRECTION ( 'NONE',  ( 1.000000000000000000, 0.000000000000000000, 0.000000000000000000 ) ) ;
#277 = CARTESIAN_POINT ( 'NONE',  ( -61.56765823437498142, 13.93229166632526805, 0.7511620957034663704 ) ) ;
#278 = CARTESIAN_POINT ( 'NONE',  ( -62.86468353124998742, 9.723958332991934128, 1.999225269531025972 ) ) ;
#279 = CARTESIAN_POINT ( 'NONE',  ( 0.3609765494018739029, 0.2499999999999997780, 1.888098105530058968 ) ) ;
#280 = CARTESIAN_POINT ( 'NONE',  ( -61.13531646874998415, 9.911458332991935904, 1.000774730468978468 ) ) ;
#281 = CARTESIAN_POINT ( 'NONE',  ( -62.49999999999998579, 12.08333333333333393, 0.6339745962155627357 ) ) ;
#282 = ORIENTED_EDGE ( 'NONE', *, *, #3450, .T. ) ;
#283 = EDGE_CURVE ( 'NONE', #10857, #3037, #6901, .T. ) ;
#284 = VECTOR ( 'NONE', #526, 1000.000000000000000 ) ;
#285 = FACE_BOUND ( 'NONE', #5927, .T. ) ;
#286 = CARTESIAN_POINT ( 'NONE',  ( -60.99999999999998579, 12.98958333265053611, 0.9226497308103762673 ) ) ;
#287 = ADVANCED_FACE ( 'NONE', ( #6844 ), #3445, .T. ) ;
#288 = CARTESIAN_POINT ( 'NONE',  ( -62.26794919243111082, 10.04241454900183328, 0.5000000000000013323 ) ) ;
#289 = CARTESIAN_POINT ( 'NONE',  ( -61.99999999999998579, 12.14062499965860198, 0.5015494609379544944 ) ) ;
#290 = CARTESIAN_POINT ( 'NONE',  ( -61.99999999999999289, 8.890624999658601979, 0.5015494609379544944 ) ) ;
#291 = CARTESIAN_POINT ( 'NONE',  ( -49.99999999999998579, -14.00000000000001243, 0.000000000000000000 ) ) ;
#292 = VERTEX_POINT ( 'NONE', #997 ) ;
#293 = CARTESIAN_POINT ( 'NONE',  ( -60.99999999999998579, 15.97916666666666607, 2.077350269189628840 ) ) ;
#294 = CARTESIAN_POINT ( 'NONE',  ( -61.13531646874997705, 10.41145833299193413, 1.000774730468978468 ) ) ;
#295 = DIRECTION ( 'NONE',  ( 1.000000000000000000, 0.000000000000000000, 0.000000000000000000 ) ) ;
#296 = CARTESIAN_POINT ( 'NONE',  ( -61.56765823437498142, 15.61979166632526628, 0.7511620957034663704 ) ) ;
#297 = ADVANCED_FACE ( 'NONE', ( #7844 ), #6003, .T. ) ;
#298 = CARTESIAN_POINT ( 'NONE',  ( -60.99999999999998579, 14.48958333265053788, 0.9226497308103762673 ) ) ;
#299 = FACE_BOUND ( 'NONE', #9767, .T. ) ;
#300 = ORIENTED_EDGE ( 'NONE', *, *, #8132, .F. ) ;
#301 = CYLINDRICAL_SURFACE ( 'NONE', #3236, 0.9999999999999981126 ) ;
#302 = VERTEX_POINT ( 'NONE', #9 ) ;
#303 = CARTESIAN_POINT ( 'NONE',  ( -61.56765823437498852, 12.78645833299193413, 2.248837904296538515 ) ) ;
#304 = CARTESIAN_POINT ( 'NONE',  ( -61.56765823437498142, 8.619791666325268054, 0.7511620957034663704 ) ) ;
#305 = CARTESIAN_POINT ( 'NONE',  ( -61.49999999999998579, 15.54166666666666607, 0.6339745962155628467 ) ) ;
#306 = ORIENTED_EDGE ( 'NONE', *, *, #5403, .T. ) ;
#307 = CARTESIAN_POINT ( 'NONE',  ( -61.99999999999998579, 12.18750000000000000, 2.654700538379254571 ) ) ;
#308 = LINE ( 'NONE', #2873, #10328 ) ;
#309 = CARTESIAN_POINT ( 'NONE',  ( -62.86468353124998032, 13.99479166632526983, 1.000774730468978246 ) ) ;
#310 = PLANE ( 'NONE',  #5287 ) ;
#311 = CARTESIAN_POINT ( 'NONE',  ( -61.49999999999998579, 10.26041666598387003, 0.6339745962155628467 ) ) ;
#312 = VERTEX_POINT ( 'NONE', #9336 ) ;
#313 = CARTESIAN_POINT ( 'NONE',  ( -105.0000000000000000, -2.500000000000000000, 4.000000000000000000 ) ) ;
#314 = CARTESIAN_POINT ( 'NONE',  ( -60.99999999999998579, 9.989583332650536107, 0.9226497308103762673 ) ) ;
#315 = CARTESIAN_POINT ( 'NONE',  ( -61.99999999999998579, 12.89062499965860376, 0.5015494609379544944 ) ) ;
#316 = ADVANCED_FACE ( 'NONE', ( #9447 ), #3389, .T. ) ;
#317 = CARTESIAN_POINT ( 'NONE',  ( -61.49999999999998579, 15.95833333333333215, 2.366025403784441927 ) ) ;
#318 =( BOUNDED_CURVE ( )  B_SPLINE_CURVE ( 2, ( #338, #1054, #8015, #9617, #7841, #6343, #2731, #6291, #1116 ),
 .UNSPECIFIED., .F., .T. ) 
 B_SPLINE_CURVE_WITH_KNOTS ( ( 3, 2, 2, 2, 3 ),
 ( 0.1953124999999999722, 0.1979166666666666574, 0.2031250000000000000, 0.2083333333333333426, 0.2109375000000000000 ),
 .UNSPECIFIED. ) 
 CURVE ( )  GEOMETRIC_REPRESENTATION_ITEM ( )  RATIONAL_B_SPLINE_CURVE ( ( 0.9330127018922194093, 0.9330127018922186322, 1.000000000000000000, 0.8660254037844387076, 1.000000000000000000, 0.8660254037844387076, 1.000000000000000000, 0.9330127018922194093, 0.9330127018922194093 ) ) 
 REPRESENTATION_ITEM ( '' )  );
#319 = EDGE_LOOP ( 'NONE', ( #4285, #2336, #2477, #10429 ) ) ;
#320 = EDGE_CURVE ( 'NONE', #4602, #5526, #6439, .T. ) ;
#321 = CARTESIAN_POINT ( 'NONE',  ( -61.99999999999998579, 10.20312499965860198, 0.5015494609379544944 ) ) ;
#322 = CARTESIAN_POINT ( 'NONE',  ( 0.000000000000000000, 0.000000000000000000, 0.000000000000000000 ) ) ;
#323 = CARTESIAN_POINT ( 'NONE',  ( -61.56765823437498852, 14.34895833299193413, 2.248837904296538515 ) ) ;
#324 = DIRECTION ( 'NONE',  ( 1.000000000000000000, 2.478176394252581387E-17, 0.000000000000000000 ) ) ;
#325 = EDGE_LOOP ( 'NONE', ( #10518, #10319, #10166, #3050 ) ) ;
#326 = CARTESIAN_POINT ( 'NONE',  ( 195.0000000000000000, -2.500000000000000000, 2.000000000000000000 ) ) ;
#327 = AXIS2_PLACEMENT_3D ( 'NONE', #3024, #4508, #7911 ) ;
#328 = CIRCLE ( 'NONE', #5652, 1.000000000000000888 ) ;
#329 = ORIENTED_EDGE ( 'NONE', *, *, #3272, .T. ) ;
#330 = CARTESIAN_POINT ( 'NONE',  ( -49.99998799999998766, -10.00000000000001066, 5.282956808509874826E-15 ) ) ;
#331 = CARTESIAN_POINT ( 'NONE',  ( -60.99999999999998579, 8.000000000000000000, 1.500000000000002220 ) ) ;
#332 = LINE ( 'NONE', #9669, #6281 ) ;
#333 = DIRECTION ( 'NONE',  ( 0.9961946980917455452, 0.000000000000000000, -0.08715574274765848506 ) ) ;
#334 = DIRECTION ( 'NONE',  ( 1.000000000000000000, 0.000000000000000000, 0.000000000000000000 ) ) ;
#335 = CARTESIAN_POINT ( 'NONE',  ( -62.86468353124999453, 14.26562499965860020, 1.500000000000002220 ) ) ;
#336 = CARTESIAN_POINT ( 'NONE',  ( -61.13531646874998415, 10.32812499965860198, 1.500000000000002220 ) ) ;
#337 = CARTESIAN_POINT ( 'NONE',  ( -61.99999999999998579, 13.28124999931720041, 0.5000000000000013323 ) ) ;
#338 = CARTESIAN_POINT ( 'NONE',  ( -61.99999999999998579, 9.562500000000000000, 0.5000000000000013323 ) ) ;
#339 = EDGE_CURVE ( 'NONE', #1405, #2680, #6609, .T. ) ;
#340 = CARTESIAN_POINT ( 'NONE',  ( -62.86468353124998742, 10.78645833299193413, 1.999225269531025972 ) ) ;
#341 = VECTOR ( 'NONE', #8505, 1000.000000000000000 ) ;
#342 = DIRECTION ( 'NONE',  ( 0.000000000000000000, 0.000000000000000000, 1.000000000000000000 ) ) ;
#343 = ORIENTED_EDGE ( 'NONE', *, *, #5169, .T. ) ;
#344 = CARTESIAN_POINT ( 'NONE',  ( 0.3612935698783895644, -0.2499999999999997224, -1.888152147991466023 ) ) ;
#345 = CARTESIAN_POINT ( 'NONE',  ( 0.6000000000000000888, 0.000000000000000000, 1.336466033005844434 ) ) ;
#346 = AXIS2_PLACEMENT_3D ( 'NONE', #4920, #5760, #10085 ) ;
#347 = ORIENTED_EDGE ( 'NONE', *, *, #4046, .F. ) ;
#348 = CARTESIAN_POINT ( 'NONE',  ( -61.13531646874998415, 8.140624999658601979, 1.500000000000002220 ) ) ;
#349 = CARTESIAN_POINT ( 'NONE',  ( -61.13531646874998415, 12.55729166632526805, 1.999225269531026417 ) ) ;
#350 = CARTESIAN_POINT ( 'NONE',  ( -61.56765823437498852, 8.786458332991934128, 2.248837904296538515 ) ) ;
#351 =( GEOMETRIC_REPRESENTATION_CONTEXT ( 3 ) GLOBAL_UNCERTAINTY_ASSIGNED_CONTEXT ( ( #4611 ) ) GLOBAL_UNIT_ASSIGNED_CONTEXT ( ( #2122, #3664, #4613 ) ) REPRESENTATION_CONTEXT ( 'NONE', 'WORKASPACE' ) );
#352 = FILL_AREA_STYLE_COLOUR ( '', #7255 ) ;
#353 = VERTEX_POINT ( 'NONE', #8565 ) ;
#354 = DIRECTION ( 'NONE',  ( -0.000000000000000000, -1.000000000000000000, -0.000000000000000000 ) ) ;
#355 = CARTESIAN_POINT ( 'NONE',  ( -61.99999999999999289, 10.32812499965860198, 2.498450539062049724 ) ) ;
#356 = CARTESIAN_POINT ( 'NONE',  ( 145.0000000000000284, -5.499999999999998224, 7.300000000000007816 ) ) ;
#357 = CARTESIAN_POINT ( 'NONE',  ( -62.43234176562499016, 14.74479166632526805, 2.248837904296538071 ) ) ;
#358 = VECTOR ( 'NONE', #7829, 1000.000000000000000 ) ;
#359 = CARTESIAN_POINT ( 'NONE',  ( -60.99999999999998579, 13.94791666598387003, 2.077350269189628840 ) ) ;
#360 = CYLINDRICAL_SURFACE ( 'NONE', #3974, 0.9999999999999981126 ) ;
#361 = ORIENTED_EDGE ( 'NONE', *, *, #10949, .T. ) ;
#362 = EDGE_CURVE ( 'NONE', #4689, #5869, #2786, .T. ) ;
#363 = CARTESIAN_POINT ( 'NONE',  ( -61.99999999999998579, 16.00000000000000000, 1.500000000000002220 ) ) ;
#364 = EDGE_LOOP ( 'NONE', ( #89, #5630 ) ) ;
#365 = STYLED_ITEM ( 'NONE', ( #4697 ), #179 ) ;
#366 = CARTESIAN_POINT ( 'NONE',  ( -61.13531646874998415, 12.57812499965860198, 1.500000000000002220 ) ) ;
#367 = EDGE_CURVE ( 'NONE', #1845, #302, #9832, .T. ) ;
#368 = CARTESIAN_POINT ( 'NONE',  ( -62.43234176562499016, 8.994791666325268054, 2.248837904296538071 ) ) ;
#369 = CARTESIAN_POINT ( 'NONE',  ( -62.99999999999998579, 10.59374999931720396, 1.500000000000001998 ) ) ;
#370 = EDGE_LOOP ( 'NONE', ( #10927, #3084, #707, #1709 ) ) ;
#371 = CARTESIAN_POINT ( 'NONE',  ( -62.99999999999998579, 12.87500000000000178, 1.500000000000001998 ) ) ;
#372 = DIRECTION ( 'NONE',  ( -1.000000000000000000, 0.000000000000000000, 0.000000000000000000 ) ) ;
#373 = CARTESIAN_POINT ( 'NONE',  ( -61.13531646874998415, 14.64062499965860020, 1.500000000000002220 ) ) ;
#374 = CARTESIAN_POINT ( 'NONE',  ( -62.26794919243111082, 13.92633545031537068, 2.500000000000003109 ) ) ;
#375 = CARTESIAN_POINT ( 'NONE',  ( -61.49999999999998579, 11.26041666598387003, 0.6339745962155628467 ) ) ;
#376 = ORIENTED_EDGE ( 'NONE', *, *, #2316, .F. ) ;
#377 = CARTESIAN_POINT ( 'NONE',  ( -114.9999999999999289, -7.999999999999998224, -2.000000000000000000 ) ) ;
#378 = CYLINDRICAL_SURFACE ( 'NONE', #125, 1.000000000000000888 ) ;
#379 = CARTESIAN_POINT ( 'NONE',  ( -61.13531646874998415, 12.30729166632526628, 1.999225269531026417 ) ) ;
#380 = LINE ( 'NONE', #7160, #836 ) ;
#381 = VERTEX_POINT ( 'NONE', #7734 ) ;
#382 = CARTESIAN_POINT ( 'NONE',  ( -61.13531646874998415, 10.14062499965860198, 1.500000000000002220 ) ) ;
#383 = CYLINDRICAL_SURFACE ( 'NONE', #5279, 0.9999999999999981126 ) ;
#384 = CARTESIAN_POINT ( 'NONE',  ( -62.86468353124999453, 14.76562499965860020, 1.500000000000002220 ) ) ;
#385 = DIRECTION ( 'NONE',  ( -0.000000000000000000, -1.000000000000000000, -0.000000000000000000 ) ) ;
#386 = VERTEX_POINT ( 'NONE', #1056 ) ;
#387 = CARTESIAN_POINT ( 'NONE',  ( 1.299999999999999156, 0.000000000000000000, 0.000000000000000000 ) ) ;
#388 = EDGE_CURVE ( 'NONE', #8021, #5388, #10231, .T. ) ;
#389 =( BOUNDED_CURVE ( )  B_SPLINE_CURVE ( 2, ( #8655, #9486, #5983, #9430, #1883, #5039, #9376, #1038, #1666 ),
 .UNSPECIFIED., .F., .F. ) 
 B_SPLINE_CURVE_WITH_KNOTS ( ( 3, 2, 2, 2, 3 ),
 ( 0.6484375000000000000, 0.6510416666666666297, 0.6562500000000000000, 0.6614583333333333703, 0.6640625000000000000 ),
 .UNSPECIFIED. ) 
 CURVE ( )  GEOMETRIC_REPRESENTATION_ITEM ( )  RATIONAL_B_SPLINE_CURVE ( ( 0.9330127018922194093, 0.9330127018922194093, 1.000000000000000000, 0.8660254037844387076, 1.000000000000000000, 0.8660254037844387076, 1.000000000000000000, 0.9330127018922194093, 0.9330127018922194093 ) ) 
 REPRESENTATION_ITEM ( '' )  );
#390 = AXIS2_PLACEMENT_3D ( 'NONE', #8453, #10271, #7624 ) ;
#391 = ORIENTED_EDGE ( 'NONE', *, *, #9319, .T. ) ;
#392 = DIRECTION ( 'NONE',  ( 0.000000000000000000, 5.282956808509869699E-16, 1.000000000000000000 ) ) ;
#393 = CARTESIAN_POINT ( 'NONE',  ( -60.99999999999998579, 8.479166666666666075, 2.077350269189628840 ) ) ;
#394 = CARTESIAN_POINT ( 'NONE',  ( -62.26794919243111082, 9.645085449632574637, 2.500000000000006217 ) ) ;
#395 = CARTESIAN_POINT ( 'NONE',  ( -61.99999999999998579, 14.28124999931720218, 0.5000000000000013323 ) ) ;
#396 = DIRECTION ( 'NONE',  ( -1.000000000000000000, -0.000000000000000000, -0.000000000000000000 ) ) ;
#397 = CARTESIAN_POINT ( 'NONE',  ( -62.86468353124999453, 14.78645833299193058, 1.999225269531025750 ) ) ;
#398 = CARTESIAN_POINT ( 'NONE',  ( -62.43234176562498305, 10.16145833299193413, 0.7511620957034662593 ) ) ;
#399 = PRODUCT_DEFINITION_CONTEXT ( 'detailed design', #1660, 'design' ) ;
#400 = CARTESIAN_POINT ( 'NONE',  ( -62.99999999999998579, 11.36458333265053611, 2.077350269189627952 ) ) ;
#401 = DIRECTION ( 'NONE',  ( -1.000000000000000000, 0.000000000000000000, 0.000000000000000000 ) ) ;
#402 = CIRCLE ( 'NONE', #212, 1.099999999999989875 ) ;
#403 = CARTESIAN_POINT ( 'NONE',  ( -61.13531646874998415, 11.14062499965860020, 1.500000000000002220 ) ) ;
#404 = DIRECTION ( 'NONE',  ( 0.000000000000000000, 0.000000000000000000, 1.000000000000000000 ) ) ;
#405 = ORIENTED_EDGE ( 'NONE', *, *, #8852, .F. ) ;
#406 = DIRECTION ( 'NONE',  ( 1.734723475976807094E-15, -1.000000000000000000, 0.000000000000000000 ) ) ;
#407 = UNCERTAINTY_MEASURE_WITH_UNIT (LENGTH_MEASURE( 1.000000000000000082E-05 ), #5246, 'distance_accuracy_value', 'NONE');
#408 = FACE_OUTER_BOUND ( 'NONE', #9322, .T. ) ;
#409 = EDGE_LOOP ( 'NONE', ( #9606, #6475, #9228, #1255, #10309, #5081, #6466, #4394, #2415, #6355, #391, #7202, #777, #5042 ) ) ;
#410 = VECTOR ( 'NONE', #7808, 1000.000000000000000 ) ;
#411 = CARTESIAN_POINT ( 'NONE',  ( -61.73205080756886787, 10.16741454900183150, 2.500000000000004885 ) ) ;
#412 = EDGE_CURVE ( 'NONE', #7538, #2208, #10852, .T. ) ;
#413 = CARTESIAN_POINT ( 'NONE',  ( -61.13531646874998415, 12.84895833299193413, 1.000774730468978468 ) ) ;
#414 = VECTOR ( 'NONE', #2699, 1000.000000000000000 ) ;
#415 = CARTESIAN_POINT ( 'NONE',  ( -61.56765823437498142, 10.61979166632526805, 0.7511620957034663704 ) ) ;
#416 = CARTESIAN_POINT ( 'NONE',  ( -61.99999999999998579, 16.00000000000000000, 0.5000000000000041078 ) ) ;
#417 = ORIENTED_EDGE ( 'NONE', *, *, #855, .T. ) ;
#418 = CARTESIAN_POINT ( 'NONE',  ( -60.99999999999998579, 8.468749999317202182, 1.500000000000002220 ) ) ;
#419 = CARTESIAN_POINT ( 'NONE',  ( -61.13531646874998415, 11.14062499965860020, 1.500000000000002220 ) ) ;
#420 = DIRECTION ( 'NONE',  ( 1.000000000000000000, 0.000000000000000000, 0.000000000000000000 ) ) ;
#421 = CARTESIAN_POINT ( 'NONE',  ( -61.99999999999998579, 14.76562499965859843, 2.498450539062049724 ) ) ;
#422 = CARTESIAN_POINT ( 'NONE',  ( -60.99999999999998579, 15.19791666598387181, 2.077350269189628840 ) ) ;
#423 = DIRECTION ( 'NONE',  ( 1.000000000000000000, 0.000000000000000000, 0.000000000000000000 ) ) ;
#424 = VERTEX_POINT ( 'NONE', #4552 ) ;
#425 = AXIS2_PLACEMENT_3D ( 'NONE', #5057, #4070, #1572 ) ;
#426 = DIRECTION ( 'NONE',  ( 0.000000000000000000, -0.000000000000000000, -1.000000000000000000 ) ) ;
#427 = VERTEX_POINT ( 'NONE', #7181 ) ;
#428 = CARTESIAN_POINT ( 'NONE',  ( -61.56765823437498852, 13.28645833299193413, 2.248837904296538515 ) ) ;
#429 = DIRECTION ( 'NONE',  ( -0.000000000000000000, -1.000000000000000000, -0.000000000000000000 ) ) ;
#430 = CARTESIAN_POINT ( 'NONE',  ( -104.9999999999999289, -16.54248688935409106, -2.000000000000000000 ) ) ;
#431 = ORIENTED_EDGE ( 'NONE', *, *, #7584, .F. ) ;
#432 = CARTESIAN_POINT ( 'NONE',  ( -60.99999999999998579, 12.50000000000000000, 1.500000000000002220 ) ) ;
#433 = AXIS2_PLACEMENT_3D ( 'NONE', #10103, #729, #1616 ) ;
#434 = CARTESIAN_POINT ( 'NONE',  ( -60.99999999999998579, 15.94791666598386826, 2.077350269189628840 ) ) ;
#435 = SURFACE_STYLE_USAGE ( .BOTH. , #2987 ) ;
#436 = CARTESIAN_POINT ( 'NONE',  ( -62.99999999999998579, 14.36458333265053611, 2.077350269189627952 ) ) ;
#437 = CARTESIAN_POINT ( 'NONE',  ( -62.99999999999998579, 10.86458333265053611, 2.077350269189627952 ) ) ;
#438 = ORIENTED_EDGE ( 'NONE', *, *, #7786, .T. ) ;
#439 = CARTESIAN_POINT ( 'NONE',  ( -61.99999999999998579, 8.000000000000000000, 1.500000000000002220 ) ) ;
#440 = CARTESIAN_POINT ( 'NONE',  ( -62.86468353124999453, 12.95312499965860198, 1.500000000000002220 ) ) ;
#441 = FILL_AREA_STYLE ('',( #3766 ) ) ;
#442 = ORIENTED_EDGE ( 'NONE', *, *, #9663, .T. ) ;
#443 = CARTESIAN_POINT ( 'NONE',  ( -61.56765823437498142, 10.68229166632526805, 0.7511620957034663704 ) ) ;
#444 = CARTESIAN_POINT ( 'NONE',  ( -62.26794919243111082, 12.54241454900183150, 0.5000000000000013323 ) ) ;
#445 = EDGE_CURVE ( 'NONE', #6076, #9310, #10674, .T. ) ;
#446 = CARTESIAN_POINT ( 'NONE',  ( -62.43234176562498305, 15.47395833299193590, 0.7511620957034662593 ) ) ;
#447 = CARTESIAN_POINT ( 'NONE',  ( -61.73205080756885366, 9.020085449632572860, 0.5000000000000028866 ) ) ;
#448 = ORIENTED_EDGE ( 'NONE', *, *, #4377, .F. ) ;
#449 = DIRECTION ( 'NONE',  ( 0.000000000000000000, 0.000000000000000000, 1.000000000000000000 ) ) ;
#450 = ORIENTED_EDGE ( 'NONE', *, *, #772, .T. ) ;
#451 = CARTESIAN_POINT ( 'NONE',  ( -49.99999999999998579, -8.000000000000000000, 0.000000000000000000 ) ) ;
#452 = CARTESIAN_POINT ( 'NONE',  ( -62.49999999999998579, 9.416666666666666075, 2.366025403784441483 ) ) ;
#453 = DIRECTION ( 'NONE',  ( -1.000000000000000000, 0.000000000000000000, -0.000000000000000000 ) ) ;
#454 = DIRECTION ( 'NONE',  ( 1.000000000000000000, 0.000000000000000000, 0.000000000000000000 ) ) ;
#455 = CARTESIAN_POINT ( 'NONE',  ( -61.99999999999998579, 8.937500000000001776, 2.500000000000002665 ) ) ;
#456 = CARTESIAN_POINT ( 'NONE',  ( -61.56765823437498142, 9.869791666325268054, 0.7511620957034663704 ) ) ;
#457 = CARTESIAN_POINT ( 'NONE',  ( -49.99999999999998579, -2.500000000000000444, 83.15773105863907233 ) ) ;
#458 = CARTESIAN_POINT ( 'NONE',  ( -62.49999999999998579, 8.302083332650536107, 0.6339745962155627357 ) ) ;
#459 = CARTESIAN_POINT ( 'NONE',  ( -62.86468353124998032, 10.49479166632526983, 1.000774730468978246 ) ) ;
#460 = DIRECTION ( 'NONE',  ( -1.000000000000000000, 0.000000000000000000, 0.000000000000000000 ) ) ;
#461 = EDGE_LOOP ( 'NONE', ( #7760, #1425, #10364, #3402 ) ) ;
#462 = CARTESIAN_POINT ( 'NONE',  ( -105.0000000000000000, 2.500000000000000000, 3.000000000000000000 ) ) ;
#463 = CARTESIAN_POINT ( 'NONE',  ( -62.26794919243111082, 9.073664549684631098, 0.5000000000000013323 ) ) ;
#464 = EDGE_LOOP ( 'NONE', ( #3656, #644 ) ) ;
#465 = CARTESIAN_POINT ( 'NONE',  ( 7.300000000000000711, 0.000000000000000000, 0.000000000000000000 ) ) ;
#466 = EDGE_CURVE ( 'NONE', #3158, #5222, #8079, .T. ) ;
#467 = CARTESIAN_POINT ( 'NONE',  ( -61.13531646874998415, 12.05729166632526628, 1.999225269531026417 ) ) ;
#468 = CARTESIAN_POINT ( 'NONE',  ( -62.86468353124999453, 10.20312499965860198, 1.500000000000002220 ) ) ;
#469 = DIRECTION ( 'NONE',  ( 1.000000000000000000, 0.000000000000000000, 0.000000000000000000 ) ) ;
#470 = VERTEX_POINT ( 'NONE', #8792 ) ;
#471 = CARTESIAN_POINT ( 'NONE',  ( -62.49999999999998579, 10.88541666598386826, 2.366025403784441483 ) ) ;
#472 = CARTESIAN_POINT ( 'NONE',  ( -62.86468353124999453, 11.28645833299193590, 1.999225269531025750 ) ) ;
#473 = EDGE_CURVE ( 'NONE', #4413, #2594, #6911, .T. ) ;
#474 = SHAPE_DEFINITION_REPRESENTATION ( #8222, #2752 ) ;
#475 = CARTESIAN_POINT ( 'NONE',  ( -62.43234176562499016, 15.99479166632526628, 2.248837904296538071 ) ) ;
#476 = CARTESIAN_POINT ( 'NONE',  ( -60.99999999999998579, 14.21874999931720218, 1.500000000000002220 ) ) ;
#477 = CARTESIAN_POINT ( 'NONE',  ( 0.000000000000000000, -2.500000000000000000, 3.000000000000000000 ) ) ;
#478 = ORIENTED_EDGE ( 'NONE', *, *, #3539, .T. ) ;
#479 = EDGE_CURVE ( 'NONE', #827, #9464, #8846, .T. ) ;
#480 = EDGE_LOOP ( 'NONE', ( #9268, #1387, #10634, #9863 ) ) ;
#481 = CARTESIAN_POINT ( 'NONE',  ( -62.43234176562498305, 13.41145833299193413, 0.7511620957034662593 ) ) ;
#482 = FACE_OUTER_BOUND ( 'NONE', #8139, .T. ) ;
#483 = DIRECTION ( 'NONE',  ( 0.000000000000000000, 0.000000000000000000, 1.000000000000000000 ) ) ;
#484 = VERTEX_POINT ( 'NONE', #2961 ) ;
#485 = CARTESIAN_POINT ( 'NONE',  ( -62.99999999999998579, 12.85416666666666607, 0.9226497308103756012 ) ) ;
#486 = CARTESIAN_POINT ( 'NONE',  ( -62.99999999999998579, 13.36458333265053433, 2.077350269189627952 ) ) ;
#487 = LINE ( 'NONE', #3873, #692 ) ;
#488 = CARTESIAN_POINT ( 'NONE',  ( -62.49999999999998579, 10.88541666598386826, 2.366025403784441483 ) ) ;
#489 = ORIENTED_EDGE ( 'NONE', *, *, #8078, .F. ) ;
#490 = ADVANCED_FACE ( 'NONE', ( #2126 ), #1118, .F. ) ;
#491 = CARTESIAN_POINT ( 'NONE',  ( -62.49999999999998579, 14.83333333333333393, 0.6339745962155627357 ) ) ;
#492 =( BOUNDED_CURVE ( )  B_SPLINE_CURVE ( 2, ( #3999, #2659, #9428, #769, #3480, #1604, #9318, #6668, #43 ),
 .UNSPECIFIED., .F., .F. ) 
 B_SPLINE_CURVE_WITH_KNOTS ( ( 3, 2, 2, 2, 3 ),
 ( 0.9765625000000000000, 0.9791666666666666297, 0.9843750000000000000, 0.9895833333333333703, 0.9921875000000000000 ),
 .UNSPECIFIED. ) 
 CURVE ( )  GEOMETRIC_REPRESENTATION_ITEM ( )  RATIONAL_B_SPLINE_CURVE ( ( 0.9330127018922194093, 0.9330127018922194093, 1.000000000000000000, 0.8660254037844387076, 1.000000000000000000, 0.8660254037844387076, 1.000000000000000000, 0.9330127018922194093, 0.9330127018922194093 ) ) 
 REPRESENTATION_ITEM ( '' )  );
#493 = CARTESIAN_POINT ( 'NONE',  ( -61.56765823437498852, 12.03645833299193413, 2.248837904296538515 ) ) ;
#494 = SURFACE_STYLE_FILL_AREA ( #10543 ) ;
#495 = ORIENTED_EDGE ( 'NONE', *, *, #4274, .T. ) ;
#496 = CARTESIAN_POINT ( 'NONE',  ( -62.86468353124999453, 11.76562499965860198, 1.500000000000002220 ) ) ;
#497 = EDGE_CURVE ( 'NONE', #2222, #3158, #7324, .T. ) ;
#498 = LINE ( 'NONE', #8221, #3700 ) ;
#499 = COLOUR_RGB ( '',0.8941176470588234615, 0.8941176470588234615, 0.8941176470588234615 ) ;
#500 = CARTESIAN_POINT ( 'NONE',  ( -62.86468353124999453, 16.01562499965860198, 1.500000000000002220 ) ) ;
#501 = CARTESIAN_POINT ( 'NONE',  ( -78.99999999999998579, 11.49999999999999645, 8.000000000000000000 ) ) ;
#502 = ORIENTED_EDGE ( 'NONE', *, *, #6812, .F. ) ;
#503 = ADVANCED_FACE ( 'NONE', ( #6406 ), #2069, .T. ) ;
#504 = DIRECTION ( 'NONE',  ( 0.000000000000000000, 0.000000000000000000, -1.000000000000000000 ) ) ;
#505 = VECTOR ( 'NONE', #9411, 1000.000000000000000 ) ;
#506 = VERTEX_POINT ( 'NONE', #4670 ) ;
#507 = CARTESIAN_POINT ( 'NONE',  ( -60.99999999999998579, 8.697916665983868256, 2.077350269189628840 ) ) ;
#508 = EDGE_CURVE ( 'NONE', #7478, #5442, #2848, .T. ) ;
#509 = CARTESIAN_POINT ( 'NONE',  ( -60.99999999999998579, 10.27083333333333393, 0.9226497308103762673 ) ) ;
#510 = LINE ( 'NONE', #9841, #4674 ) ;
#511 = CARTESIAN_POINT ( 'NONE',  ( 150.0000000000000000, -2.500000000000000444, 6.000000000000000000 ) ) ;
#512 = DIRECTION ( 'NONE',  ( 0.000000000000000000, 1.000000000000000000, 0.000000000000000000 ) ) ;
#513 = CARTESIAN_POINT ( 'NONE',  ( -62.49999999999998579, 8.385416665983870033, 2.366025403784441483 ) ) ;
#514 = COLOUR_RGB ( '',0.8941176470588234615, 0.8941176470588234615, 0.8941176470588234615 ) ;
#515 = CARTESIAN_POINT ( 'NONE',  ( -61.56765823437498142, 12.43229166632526805, 0.7511620957034663704 ) ) ;
#516 = CARTESIAN_POINT ( 'NONE',  ( -62.49999999999998579, 13.58333333333333215, 0.6339745962155627357 ) ) ;
#517 = ORIENTED_EDGE ( 'NONE', *, *, #8212, .T. ) ;
#518 = LINE ( 'NONE', #6516, #873 ) ;
#519 = CARTESIAN_POINT ( 'NONE',  ( -61.99999999999998579, 9.187500000000000000, 2.500000000000002665 ) ) ;
#520 = AXIS2_PLACEMENT_3D ( 'NONE', #5380, #396, #3722 ) ;
#521 = ORIENTED_EDGE ( 'NONE', *, *, #9600, .F. ) ;
#522 = CARTESIAN_POINT ( 'NONE',  ( -61.99999999999998579, 16.00000000000000000, 1.500000000000002220 ) ) ;
#523 = CARTESIAN_POINT ( 'NONE',  ( -62.86468353124998742, 13.72395833299193413, 1.999225269531025972 ) ) ;
#524 = CIRCLE ( 'NONE', #4765, 25.99999999999999645 ) ;
#525 = CARTESIAN_POINT ( 'NONE',  ( -61.13531646874997705, 10.84895833299193413, 1.000774730468978468 ) ) ;
#526 = DIRECTION ( 'NONE',  ( 0.000000000000000000, -1.000000000000000000, 0.000000000000000000 ) ) ;
#527 = ORIENTED_EDGE ( 'NONE', *, *, #2808, .T. ) ;
#528 = CARTESIAN_POINT ( 'NONE',  ( -120.0000000000000000, -4.000000000000019540, 0.000000000000000000 ) ) ;
#529 = CARTESIAN_POINT ( 'NONE',  ( -62.43234176562498305, 10.97395833299193590, 0.7511620957034662593 ) ) ;
#530 = SHAPE_DEFINITION_REPRESENTATION ( #1480, #9271 ) ;
#531 = DIRECTION ( 'NONE',  ( -1.000000000000000000, 0.000000000000000000, 0.000000000000000000 ) ) ;
#532 = CARTESIAN_POINT ( 'NONE',  ( -61.99999999999998579, 15.40624999931720218, 2.654700538379254571 ) ) ;
#533 = CARTESIAN_POINT ( 'NONE',  ( -62.26794919243111082, 16.04241454900182973, 0.5000000000000013323 ) ) ;
#534 = EDGE_LOOP ( 'NONE', ( #1368, #8462, #4338, #10886 ) ) ;
#535 = EDGE_CURVE ( 'NONE', #10303, #6298, #1585, .T. ) ;
#536 = CIRCLE ( 'NONE', #1421, 40.00000000000000711 ) ;
#537 = ORIENTED_EDGE ( 'NONE', *, *, #9340, .T. ) ;
#538 = ADVANCED_FACE ( 'NONE', ( #8017 ), #3731, .F. ) ;
#539 =( GEOMETRIC_REPRESENTATION_CONTEXT ( 3 ) GLOBAL_UNCERTAINTY_ASSIGNED_CONTEXT ( ( #6697 ) ) GLOBAL_UNIT_ASSIGNED_CONTEXT ( ( #8208, #6320, #9818 ) ) REPRESENTATION_CONTEXT ( 'NONE', 'WORKASPACE' ) );
#540 = CARTESIAN_POINT ( 'NONE',  ( -61.13531646874998415, 13.07812499965860198, 1.500000000000002220 ) ) ;
#541 = CARTESIAN_POINT ( 'NONE',  ( -61.13531646874998415, 9.578124999658600203, 1.500000000000002220 ) ) ;
#542 =( REPRESENTATION_RELATIONSHIP ('NONE','NONE', #560, #8867 ) REPRESENTATION_RELATIONSHIP_WITH_TRANSFORMATION ( #4842 )SHAPE_REPRESENTATION_RELATIONSHIP( ) );
#543 = CARTESIAN_POINT ( 'NONE',  ( -61.99999999999998579, 11.81249999999999822, 0.5000000000000013323 ) ) ;
#544 = VERTEX_POINT ( 'NONE', #3013 ) ;
#545 = CARTESIAN_POINT ( 'NONE',  ( -62.49999999999998579, 13.08333333333333215, 0.6339745962155627357 ) ) ;
#546 = CARTESIAN_POINT ( 'NONE',  ( -61.99999999999998579, 8.937500000000001776, 2.500000000000002665 ) ) ;
#547 = AXIS2_PLACEMENT_3D ( 'NONE', #10152, #5041, #1715 ) ;
#548 = CARTESIAN_POINT ( 'NONE',  ( -62.99999999999998579, 11.11458333265053611, 2.077350269189627952 ) ) ;
#549 = AXIS2_PLACEMENT_3D ( 'NONE', #10284, #2972, #420 ) ;
#550 = CARTESIAN_POINT ( 'NONE',  ( -62.49999999999998579, 14.91666666666666607, 2.366025403784441483 ) ) ;
#551 = VECTOR ( 'NONE', #1388, 1000.000000000000000 ) ;
#552 = CARTESIAN_POINT ( 'NONE',  ( -61.99999999999998579, 12.26562499965860198, 2.498450539062049724 ) ) ;
#553 = CARTESIAN_POINT ( 'NONE',  ( 0.000000000000000000, 0.2499999999999982792, 2.000000000000001776 ) ) ;
#554 = ORIENTED_EDGE ( 'NONE', *, *, #5299, .F. ) ;
#555 = EDGE_CURVE ( 'NONE', #9700, #1702, #8379, .T. ) ;
#556 = CARTESIAN_POINT ( 'NONE',  ( -61.99999999999998579, 11.82812499965860198, 2.498450539062049724 ) ) ;
#557 = CARTESIAN_POINT ( 'NONE',  ( -62.99999999999998579, 12.61458333265053611, 2.077350269189627952 ) ) ;
#558 = DIRECTION ( 'NONE',  ( -0.000000000000000000, -0.000000000000000000, -1.000000000000000000 ) ) ;
#559 = ORIENTED_EDGE ( 'NONE', *, *, #4763, .T. ) ;
#560 = SHAPE_REPRESENTATION ( 'MAS-164', ( #4426, #8333, #5304, #7809, #9054, #9223, #549, #4241, #5848, #1052, #2478, #8696 ), #1951 ) ;
#561 = CARTESIAN_POINT ( 'NONE',  ( -62.99999999999998579, 11.10416666666666607, 0.9226497308103756012 ) ) ;
#562 = VERTEX_POINT ( 'NONE', #8127 ) ;
#563 = CARTESIAN_POINT ( 'NONE',  ( -62.99999999999998579, 9.822916665983871809, 0.9226497308103756012 ) ) ;
#564 = CARTESIAN_POINT ( 'NONE',  ( -62.99999999999998579, 9.125000000000000000, 1.500000000000001998 ) ) ;
#565 = CARTESIAN_POINT ( 'NONE',  ( -61.99999999999998579, 26.00000000000000355, -1.000000000000000000 ) ) ;
#566 = DIRECTION ( 'NONE',  ( -1.000000000000000000, 0.000000000000000000, 0.000000000000000000 ) ) ;
#567 = CARTESIAN_POINT ( 'NONE',  ( -149.9999999999999716, 8.000000000000000000, 3.000000000000000000 ) ) ;
#568 = DIRECTION ( 'NONE',  ( -0.000000000000000000, -1.000000000000000000, -0.000000000000000000 ) ) ;
#569 = CARTESIAN_POINT ( 'NONE',  ( -62.43234176562498305, 11.72395833299193590, 0.7511620957034662593 ) ) ;
#570 = VERTEX_POINT ( 'NONE', #3901 ) ;
#571 = LINE ( 'NONE', #7345, #5302 ) ;
#572 = EDGE_CURVE ( 'NONE', #10486, #930, #1997, .T. ) ;
#573 = DIRECTION ( 'NONE',  ( -0.000000000000000000, -0.000000000000000000, 1.000000000000000000 ) ) ;
#574 = ORIENTED_EDGE ( 'NONE', *, *, #8698, .F. ) ;
#575 = CARTESIAN_POINT ( 'NONE',  ( -60.99999999999998579, 14.21874999931720218, 1.500000000000002220 ) ) ;
#576 = CARTESIAN_POINT ( 'NONE',  ( -61.99999999999998579, 13.64062499965860198, 0.5015494609379544944 ) ) ;
#577 = CARTESIAN_POINT ( 'NONE',  ( -61.56765823437498852, 9.786458332991934128, 2.248837904296538515 ) ) ;
#578 = ORIENTED_EDGE ( 'NONE', *, *, #2504, .T. ) ;
#579 = CARTESIAN_POINT ( 'NONE',  ( -61.99999999999998579, 14.18750000000000000, 2.500000000000002665 ) ) ;
#580 = AXIS2_PLACEMENT_3D ( 'NONE', #1728, #9502, #4442 ) ;
#581 = CARTESIAN_POINT ( 'NONE',  ( -61.56765823437498142, 11.68229166632526805, 0.7511620957034663704 ) ) ;
#582 = CARTESIAN_POINT ( 'NONE',  ( -62.43234176562498305, 14.72395833299193413, 0.7511620957034662593 ) ) ;
#583 = APPLICATION_PROTOCOL_DEFINITION ( 'draft international standard', 'automotive_design', 1998, #10872 ) ;
#584 = CARTESIAN_POINT ( 'NONE',  ( -62.49999999999998579, 13.55208333265053433, 0.6339745962155627357 ) ) ;
#585 = CARTESIAN_POINT ( 'NONE',  ( -61.49999999999998579, 16.17708333265053255, 2.366025403784441927 ) ) ;
#586 = FACE_OUTER_BOUND ( 'NONE', #5446, .T. ) ;
#587 = ORIENTED_EDGE ( 'NONE', *, *, #4211, .T. ) ;
#588 = DIRECTION ( 'NONE',  ( 1.000000000000000000, 0.000000000000000000, 0.000000000000000000 ) ) ;
#589 = ADVANCED_FACE ( 'NONE', ( #5826, #10002 ), #5614, .T. ) ;
#590 = CARTESIAN_POINT ( 'NONE',  ( -60.99999999999998579, 15.23958333265053611, 0.9226497308103762673 ) ) ;
#591 = VECTOR ( 'NONE', #8546, 1000.000000000000000 ) ;
#592 = AXIS2_PLACEMENT_3D ( 'NONE', #10434, #7171, #272 ) ;
#593 = CARTESIAN_POINT ( 'NONE',  ( -61.13531646874998415, 14.07812499965860198, 1.500000000000002220 ) ) ;
#594 = CARTESIAN_POINT ( 'NONE',  ( -61.99999999999998579, 10.14062499965860198, 0.5015494609379544944 ) ) ;
#595 = CARTESIAN_POINT ( 'NONE',  ( 0.000000000000000000, 0.000000000000000000, 0.000000000000000000 ) ) ;
#596 = ORIENTED_EDGE ( 'NONE', *, *, #6504, .F. ) ;
#597 = CARTESIAN_POINT ( 'NONE',  ( -62.99999999999998579, 14.12499999999999822, 1.500000000000001998 ) ) ;
#598 = CARTESIAN_POINT ( 'NONE',  ( -61.99999999999998579, 13.40624999931720041, 2.500000000000002665 ) ) ;
#599 = AXIS2_PLACEMENT_3D ( 'NONE', #4517, #5230, #6973 ) ;
#600 = CIRCLE ( 'NONE', #9605, 1.928074011315806136 ) ;
#601 = CARTESIAN_POINT ( 'NONE',  ( -61.99999999999998579, 11.53124999931720396, 0.3452994616207497591 ) ) ;
#602 = EDGE_CURVE ( 'NONE', #6810, #5402, #2367, .T. ) ;
#603 = DIRECTION ( 'NONE',  ( 0.000000000000000000, 0.000000000000000000, -1.000000000000000000 ) ) ;
#604 = CIRCLE ( 'NONE', #9648, 1.000000000000000888 ) ;
#605 = CARTESIAN_POINT ( 'NONE',  ( -61.99999999999998579, 13.89062499965860198, 0.5015494609379544944 ) ) ;
#606 = LINE ( 'NONE', #2414, #9719 ) ;
#607 = VERTEX_POINT ( 'NONE', #3951 ) ;
#608 = CARTESIAN_POINT ( 'NONE',  ( -61.13531646874998415, 12.11979166632526628, 1.999225269531026417 ) ) ;
#609 = CARTESIAN_POINT ( 'NONE',  ( -61.99999999999998579, 16.00000000000000000, 1.500000000000002220 ) ) ;
#610 = VECTOR ( 'NONE', #6030, 1000.000000000000000 ) ;
#611 = CYLINDRICAL_SURFACE ( 'NONE', #4223, 1.099999999999989875 ) ;
#612 = EDGE_LOOP ( 'NONE', ( #5930, #4640, #8433, #5603 ) ) ;
#613 = LINE ( 'NONE', #4764, #9060 ) ;
#614 = ADVANCED_FACE ( 'NONE', ( #3275 ), #4286, .T. ) ;
#615 = EDGE_LOOP ( 'NONE', ( #230, #259, #4915, #1418 ) ) ;
#616 = CARTESIAN_POINT ( 'NONE',  ( -144.9999999999999147, -16.54248688935410883, -2.000000000000000000 ) ) ;
#617 = CARTESIAN_POINT ( 'NONE',  ( -61.49999999999998579, 9.458333333333332149, 2.366025403784441927 ) ) ;
#618 = CARTESIAN_POINT ( 'NONE',  ( -37.99999999999999289, -14.00000000000000888, -0.9999999999999947820 ) ) ;
#619 = CARTESIAN_POINT ( 'NONE',  ( -61.13531646874998415, 8.161458332991935904, 1.000774730468978468 ) ) ;
#620 = CARTESIAN_POINT ( 'NONE',  ( -61.99999999999998579, 14.90624999931720218, 2.500000000000002665 ) ) ;
#621 =( BOUNDED_CURVE ( )  B_SPLINE_CURVE ( 2, ( #8138, #7301, #6474, #4787, #7352, #7561, #3283, #6631, #630 ),
 .UNSPECIFIED., .F., .T. ) 
 B_SPLINE_CURVE_WITH_KNOTS ( ( 3, 2, 2, 2, 3 ),
 ( 0.4296875000000000555, 0.4322916666666666852, 0.4375000000000000000, 0.4427083333333333148, 0.4453125000000000000 ),
 .UNSPECIFIED. ) 
 CURVE ( )  GEOMETRIC_REPRESENTATION_ITEM ( )  RATIONAL_B_SPLINE_CURVE ( ( 0.9330127018922192983, 0.9330127018922207416, 1.000000000000000000, 0.8660254037844387076, 1.000000000000000000, 0.8660254037844387076, 1.000000000000000000, 0.9330127018922194093, 0.9330127018922194093 ) ) 
 REPRESENTATION_ITEM ( '' )  );
#622 = CARTESIAN_POINT ( 'NONE',  ( -61.99999999999998579, 8.406249999317202182, 2.654700538379254571 ) ) ;
#623 = CARTESIAN_POINT ( 'NONE',  ( -61.13531646874998415, 12.11979166632526628, 1.999225269531026417 ) ) ;
#624 = EDGE_LOOP ( 'NONE', ( #4577, #6804, #1440, #7145 ) ) ;
#625 = CARTESIAN_POINT ( 'NONE',  ( -61.99999999999998579, 8.000000000000000000, 0.5000000000000041078 ) ) ;
#626 = CARTESIAN_POINT ( 'NONE',  ( -37.99999999999999289, -14.00000000000000888, -0.9999999999999947820 ) ) ;
#627 = FACE_OUTER_BOUND ( 'NONE', #8133, .T. ) ;
#628 = CARTESIAN_POINT ( 'NONE',  ( -61.13531646874998415, 13.84895833299193413, 1.000774730468978468 ) ) ;
#629 = CARTESIAN_POINT ( 'NONE',  ( 7.300000000000000711, 0.000000000000000000, 0.000000000000000000 ) ) ;
#630 = CARTESIAN_POINT ( 'NONE',  ( -61.99999999999998579, 11.78124999931720218, 0.5000000000000013323 ) ) ;
#631 = DIRECTION ( 'NONE',  ( 0.000000000000000000, 0.000000000000000000, -1.000000000000000000 ) ) ;
#632 = CARTESIAN_POINT ( 'NONE',  ( -62.86468353124998032, 11.99479166632526628, 1.000774730468978024 ) ) ;
#633 = CARTESIAN_POINT ( 'NONE',  ( -61.56765823437498852, 15.09895833299193590, 2.248837904296538515 ) ) ;
#634 = PRODUCT_CONTEXT ( 'NONE', #9523, 'mechanical' ) ;
#635 = CARTESIAN_POINT ( 'NONE',  ( -62.43234176562498305, 8.473958332991934128, 0.7511620957034662593 ) ) ;
#636 = CARTESIAN_POINT ( 'NONE',  ( -62.49999999999998579, 10.33333333333333393, 0.6339745962155627357 ) ) ;
#637 = ORIENTED_EDGE ( 'NONE', *, *, #7042, .T. ) ;
#638 = CARTESIAN_POINT ( 'NONE',  ( -62.49999999999998579, 11.80208333265053611, 0.6339745962155627357 ) ) ;
#639 = FACE_OUTER_BOUND ( 'NONE', #8188, .T. ) ;
#640 = ADVANCED_FACE ( 'NONE', ( #10832 ), #2433, .T. ) ;
#641 = CARTESIAN_POINT ( 'NONE',  ( -62.43234176562499016, 13.74479166632526805, 2.248837904296538071 ) ) ;
#642 = CARTESIAN_POINT ( 'NONE',  ( -62.86468353124998742, 10.22395833299193413, 1.999225269531025972 ) ) ;
#643 = DIRECTION ( 'NONE',  ( 0.000000000000000000, 0.000000000000000000, -1.000000000000000000 ) ) ;
#644 = ORIENTED_EDGE ( 'NONE', *, *, #9959, .F. ) ;
#645 = CARTESIAN_POINT ( 'NONE',  ( -62.99999999999998579, 13.12500000000000178, 1.500000000000001998 ) ) ;
#646 = EDGE_CURVE ( 'NONE', #607, #3158, #4934, .T. ) ;
#647 = CARTESIAN_POINT ( 'NONE',  ( -62.49999999999998579, 13.30208333265053433, 0.6339745962155627357 ) ) ;
#648 = CARTESIAN_POINT ( 'NONE',  ( -62.99999999999998579, 11.32291666598386826, 0.9226497308103756012 ) ) ;
#649 = CARTESIAN_POINT ( 'NONE',  ( -61.56765823437498852, 14.03645833299193413, 2.248837904296538515 ) ) ;
#650 =( NAMED_UNIT ( * ) PLANE_ANGLE_UNIT ( ) SI_UNIT ( $, .RADIAN. ) );
#651 = ORIENTED_EDGE ( 'NONE', *, *, #6556, .T. ) ;
#652 = CARTESIAN_POINT ( 'NONE',  ( -61.99999999999998579, 11.45312499965860020, 0.5015494609379544944 ) ) ;
#653 = CARTESIAN_POINT ( 'NONE',  ( -60.99999999999998579, 12.21874999931720218, 1.500000000000002220 ) ) ;
#654 = CARTESIAN_POINT ( 'NONE',  ( -61.13531646874998415, 15.41145833299193413, 1.000774730468978468 ) ) ;
#655 = EDGE_LOOP ( 'NONE', ( #7806, #6596, #6590, #7819, #2641, #6040 ) ) ;
#656 = FACE_OUTER_BOUND ( 'NONE', #364, .T. ) ;
#657 = EDGE_CURVE ( 'NONE', #5688, #8551, #9953, .T. ) ;
#658 = EDGE_CURVE ( 'NONE', #5256, #1211, #1641, .T. ) ;
#659 = ORIENTED_EDGE ( 'NONE', *, *, #9592, .T. ) ;
#660 = CARTESIAN_POINT ( 'NONE',  ( -61.49999999999998579, 8.677083332650536107, 2.366025403784441927 ) ) ;
#661 = CARTESIAN_POINT ( 'NONE',  ( -62.49999999999998579, 9.166666666666666075, 2.366025403784441483 ) ) ;
#662 = CARTESIAN_POINT ( 'NONE',  ( -61.49999999999998579, 8.541666666666666075, 0.6339745962155628467 ) ) ;
#663 = CARTESIAN_POINT ( 'NONE',  ( -61.99999999999998579, 10.53124999931720396, 0.5000000000000013323 ) ) ;
#664 = CARTESIAN_POINT ( 'NONE',  ( -62.43234176562499016, 11.55729166632526805, 2.248837904296538071 ) ) ;
#665 = CARTESIAN_POINT ( 'NONE',  ( -62.26794919243111082, 14.54241454900183150, 0.5000000000000013323 ) ) ;
#666 = ORIENTED_EDGE ( 'NONE', *, *, #6256, .F. ) ;
#667 = LINE ( 'NONE', #7455, #4965 ) ;
#668 = CIRCLE ( 'NONE', #1009, 3.000000000000002665 ) ;
#669 = ORIENTED_EDGE ( 'NONE', *, *, #6090, .F. ) ;
#670 = LINE ( 'NONE', #9229, #10699 ) ;
#671 = CARTESIAN_POINT ( 'NONE',  ( -62.43234176562498305, 13.41145833299193413, 0.7511620957034662593 ) ) ;
#672 = CARTESIAN_POINT ( 'NONE',  ( -76.89999999999999147, -11.50000000000000711, -2.000000000000001332 ) ) ;
#673 = DIRECTION ( 'NONE',  ( -3.469446951953572774E-16, 1.000000000000000000, 0.000000000000000000 ) ) ;
#674 =( BOUNDED_CURVE ( )  B_SPLINE_CURVE ( 2, ( #2327, #7336, #4041, #563, #4820, #3995, #2377, #9107, #2277 ),
 .UNSPECIFIED., .F., .T. ) 
 B_SPLINE_CURVE_WITH_KNOTS ( ( 3, 2, 2, 2, 3 ),
 ( 0.1953124999999999445, 0.1979166666666666574, 0.2031250000000000000, 0.2083333333333333426, 0.2109375000000000000 ),
 .UNSPECIFIED. ) 
 CURVE ( )  GEOMETRIC_REPRESENTATION_ITEM ( )  RATIONAL_B_SPLINE_CURVE ( ( 0.9330127018922192983, 0.9330127018922178550, 1.000000000000000000, 0.8660254037844387076, 1.000000000000000000, 0.8660254037844387076, 1.000000000000000000, 0.9330127018922194093, 0.9330127018922194093 ) ) 
 REPRESENTATION_ITEM ( '' )  );
#675 = CARTESIAN_POINT ( 'NONE',  ( -62.99999999999998579, 14.10416666666666785, 0.9226497308103756012 ) ) ;
#676 = CARTESIAN_POINT ( 'NONE',  ( -61.56765823437498142, 12.43229166632526805, 0.7511620957034663704 ) ) ;
#677 = EDGE_CURVE ( 'NONE', #24, #3356, #3404, .T. ) ;
#678 = AXIS2_PLACEMENT_3D ( 'NONE', #10292, #1697, #1916 ) ;
#679 = CARTESIAN_POINT ( 'NONE',  ( -61.56765823437498142, 15.18229166632526805, 0.7511620957034663704 ) ) ;
#680 = DIRECTION ( 'NONE',  ( -0.000000000000000000, 1.000000000000000000, -0.000000000000000000 ) ) ;
#681 = CARTESIAN_POINT ( 'NONE',  ( -62.26794919243111082, 15.07366454968462932, 0.5000000000000013323 ) ) ;
#682 = CARTESIAN_POINT ( 'NONE',  ( -62.86468353124998032, 8.244791666325268054, 1.000774730468978246 ) ) ;
#683 = AXIS2_PLACEMENT_3D ( 'NONE', #6099, #5365, #6331 ) ;
#684 = CARTESIAN_POINT ( 'NONE',  ( -61.99999999999998579, 10.43750000000000000, 2.500000000000002665 ) ) ;
#685 = ORIENTED_EDGE ( 'NONE', *, *, #10440, .F. ) ;
#686 = FACE_BOUND ( 'NONE', #7136, .T. ) ;
#687 = CARTESIAN_POINT ( 'NONE',  ( 150.0000000000000284, -8.000000000000000000, 3.000000000000000000 ) ) ;
#688 = PRESENTATION_LAYER_ASSIGNMENT (  '', '', ( #6552 ) ) ;
#689 = CARTESIAN_POINT ( 'NONE',  ( -61.56765823437498142, 14.36979166632526983, 0.7511620957034663704 ) ) ;
#690 = CARTESIAN_POINT ( 'NONE',  ( -62.86468353124998032, 9.932291666325269830, 1.000774730468978246 ) ) ;
#691 = CARTESIAN_POINT ( 'NONE',  ( -61.13531646874997705, 15.16145833299193590, 1.000774730468978468 ) ) ;
#692 = VECTOR ( 'NONE', #10647, 1000.000000000000000 ) ;
#693 = DIRECTION ( 'NONE',  ( 1.000000000000000000, -0.000000000000000000, 0.000000000000000000 ) ) ;
#694 = EDGE_LOOP ( 'NONE', ( #1478, #1766 ) ) ;
#695 = CARTESIAN_POINT ( 'NONE',  ( -62.99999999999998579, 13.62500000000000000, 1.500000000000001998 ) ) ;
#696 = FACE_OUTER_BOUND ( 'NONE', #8472, .T. ) ;
#697 = EDGE_CURVE ( 'NONE', #5580, #8781, #5764, .T. ) ;
#698 = FILL_AREA_STYLE_COLOUR ( '', #3359 ) ;
#699 = VECTOR ( 'NONE', #786, 1000.000000000000000 ) ;
#700 = CARTESIAN_POINT ( 'NONE',  ( -62.49999999999998579, 12.30208333265053611, 0.6339745962155627357 ) ) ;
#701 =( NAMED_UNIT ( * ) SI_UNIT ( $, .STERADIAN. ) SOLID_ANGLE_UNIT ( ) );
#702 = MECHANICAL_DESIGN_GEOMETRIC_PRESENTATION_REPRESENTATION (  '', ( #1232 ), #9754 ) ;
#703 = EDGE_CURVE ( 'NONE', #827, #5087, #9117, .T. ) ;
#704 = CARTESIAN_POINT ( 'NONE',  ( -61.13531646874998415, 14.59895833299193590, 1.000774730468978468 ) ) ;
#705 = CARTESIAN_POINT ( 'NONE',  ( -61.73205080756886076, 11.55133545031537068, 0.5000000000000014433 ) ) ;
#706 = VECTOR ( 'NONE', #9292, 1000.000000000000000 ) ;
#707 = ORIENTED_EDGE ( 'NONE', *, *, #7222, .T. ) ;
#708 = CARTESIAN_POINT ( 'NONE',  ( -61.56765823437498142, 12.18229166632526628, 0.7511620957034663704 ) ) ;
#709 = CARTESIAN_POINT ( 'NONE',  ( -61.99999999999998579, 11.53124999931720218, 0.5000000000000013323 ) ) ;
#710 = VECTOR ( 'NONE', #6574, 1000.000000000000000 ) ;
#711 = DIRECTION ( 'NONE',  ( -0.000000000000000000, -1.000000000000000000, -0.000000000000000000 ) ) ;
#712 = EDGE_LOOP ( 'NONE', ( #5700, #5291 ) ) ;
#713 = CARTESIAN_POINT ( 'NONE',  ( -57.99999999999998579, -10.00000000000000888, 0.000000000000000000 ) ) ;
#714 = CARTESIAN_POINT ( 'NONE',  ( -61.56765823437498142, 15.36979166632526805, 0.7511620957034663704 ) ) ;
#715 = ORIENTED_EDGE ( 'NONE', *, *, #4832, .T. ) ;
#716 = FACE_OUTER_BOUND ( 'NONE', #7545, .T. ) ;
#717 = CARTESIAN_POINT ( 'NONE',  ( -62.99999999999998579, 10.60416666666666607, 0.9226497308103756012 ) ) ;
#718 = FACE_OUTER_BOUND ( 'NONE', #3346, .T. ) ;
#719 = LINE ( 'NONE', #7497, #9735 ) ;
#720 = CARTESIAN_POINT ( 'NONE',  ( -61.99999999999998579, 9.156249999317202182, 2.654700538379254571 ) ) ;
#721 = CARTESIAN_POINT ( 'NONE',  ( -62.43234176562498305, 11.97395833299193413, 0.7511620957034662593 ) ) ;
#722 = EDGE_CURVE ( 'NONE', #7043, #3002, #2720, .T. ) ;
#723 = CARTESIAN_POINT ( 'NONE',  ( -62.49999999999998579, 14.63541666598387003, 2.366025403784441483 ) ) ;
#724 = VERTEX_POINT ( 'NONE', #2548 ) ;
#725 = DIRECTION ( 'NONE',  ( -1.734723475976807094E-15, 1.000000000000000000, 0.000000000000000000 ) ) ;
#726 = ORIENTED_EDGE ( 'NONE', *, *, #10589, .F. ) ;
#727 = DIRECTION ( 'NONE',  ( 1.110223024625156540E-15, 1.000000000000000000, 0.000000000000000000 ) ) ;
#728 = CARTESIAN_POINT ( 'NONE',  ( -61.13531646874998415, 14.34895833299193413, 1.000774730468978468 ) ) ;
#729 = DIRECTION ( 'NONE',  ( 0.000000000000000000, -1.000000000000000000, 0.000000000000000000 ) ) ;
#730 = CARTESIAN_POINT ( 'NONE',  ( -149.9999999999999716, -8.000000000000000000, 0.000000000000000000 ) ) ;
#731 = CARTESIAN_POINT ( 'NONE',  ( -149.9999999999999716, 8.000000000000000000, 0.000000000000000000 ) ) ;
#732 = CARTESIAN_POINT ( 'NONE',  ( -61.13531646874998415, 13.14062499965860198, 1.500000000000002220 ) ) ;
#733 = CARTESIAN_POINT ( 'NONE',  ( -62.86468353124999453, 15.01562499965860020, 1.500000000000002220 ) ) ;
#734 = CARTESIAN_POINT ( 'NONE',  ( -120.0000000000000000, 3.999999999999980904, -2.000000000000000000 ) ) ;
#735 = CARTESIAN_POINT ( 'NONE',  ( -79.09999999999998010, -11.50000000000000711, -2.000000000000000000 ) ) ;
#736 = CARTESIAN_POINT ( 'NONE',  ( -62.49999999999998579, 15.80208333265053788, 0.6339745962155627357 ) ) ;
#737 = CARTESIAN_POINT ( 'NONE',  ( -61.99999999999998579, 16.00000000000000000, 1.500000000000002220 ) ) ;
#738 = EDGE_LOOP ( 'NONE', ( #3698, #10471 ) ) ;
#739 = DIRECTION ( 'NONE',  ( 0.000000000000000000, 0.000000000000000000, -1.000000000000000000 ) ) ;
#740 = PLANE ( 'NONE',  #6798 ) ;
#741 = EDGE_CURVE ( 'NONE', #9355, #2941, #7719, .T. ) ;
#742 =( BOUNDED_CURVE ( )  B_SPLINE_CURVE ( 2, ( #3926, #8157, #8263, #9979, #10644, #4696, #7423, #8104, #2361 ),
 .UNSPECIFIED., .F., .T. ) 
 B_SPLINE_CURVE_WITH_KNOTS ( ( 3, 2, 2, 2, 3 ),
 ( 0.3515625000000000000, 0.3541666666666666852, 0.3593750000000000000, 0.3645833333333333148, 0.3671875000000000000 ),
 .UNSPECIFIED. ) 
 CURVE ( )  GEOMETRIC_REPRESENTATION_ITEM ( )  RATIONAL_B_SPLINE_CURVE ( ( 0.9330127018922194093, 0.9330127018922194093, 1.000000000000000000, 0.8660254037844387076, 1.000000000000000000, 0.8660254037844387076, 1.000000000000000000, 0.9330127018922194093, 0.9330127018922194093 ) ) 
 REPRESENTATION_ITEM ( '' )  );
#743 = VECTOR ( 'NONE', #342, 1000.000000000000000 ) ;
#744 = CARTESIAN_POINT ( 'NONE',  ( -62.43234176562499016, 13.99479166632526805, 2.248837904296538071 ) ) ;
#745 = CARTESIAN_POINT ( 'NONE',  ( -61.13531646874998415, 9.807291666325268054, 1.999225269531026417 ) ) ;
#746 = CARTESIAN_POINT ( 'NONE',  ( -61.99999999999999289, 16.07812499965860198, 2.498450539062049724 ) ) ;
#747 = CARTESIAN_POINT ( 'NONE',  ( -61.73205080756886076, 14.41741454900183150, 2.500000000000003109 ) ) ;
#748 = ORIENTED_EDGE ( 'NONE', *, *, #4906, .F. ) ;
#749 = CARTESIAN_POINT ( 'NONE',  ( -61.99999999999998579, 13.56250000000000000, 0.3452994616207497591 ) ) ;
#750 = CARTESIAN_POINT ( 'NONE',  ( -62.43234176562498305, 9.223958332991935904, 0.7511620957034662593 ) ) ;
#751 = CARTESIAN_POINT ( 'NONE',  ( -62.49999999999998579, 11.55208333265053611, 0.6339745962155627357 ) ) ;
#752 = AXIS2_PLACEMENT_3D ( 'NONE', #1956, #4720, #7126 ) ;
#753 = CIRCLE ( 'NONE', #921, 2.000000000000000000 ) ;
#754 = CARTESIAN_POINT ( 'NONE',  ( -61.99999999999998579, 10.93750000000000000, 2.500000000000002665 ) ) ;
#755 = CARTESIAN_POINT ( 'NONE',  ( -61.13531646874998415, 13.30729166632526983, 1.999225269531026417 ) ) ;
#756 = FACE_OUTER_BOUND ( 'NONE', #3119, .T. ) ;
#757 = EDGE_LOOP ( 'NONE', ( #9977, #1342, #4104, #2542 ) ) ;
#758 = AXIS2_PLACEMENT_3D ( 'NONE', #10274, #3559, #3502 ) ;
#759 = CIRCLE ( 'NONE', #7138, 0.9999999999999983347 ) ;
#760 = CARTESIAN_POINT ( 'NONE',  ( -61.99999999999998579, 13.32812499965860198, 2.498450539062049724 ) ) ;
#761 = DIRECTION ( 'NONE',  ( -0.000000000000000000, -0.000000000000000000, 1.000000000000000000 ) ) ;
#762 = DIRECTION ( 'NONE',  ( -1.734723475976807094E-15, 1.000000000000000000, 0.000000000000000000 ) ) ;
#763 = ORIENTED_EDGE ( 'NONE', *, *, #2423, .F. ) ;
#764 = CIRCLE ( 'NONE', #5367, 1.099999999999989875 ) ;
#765 = ORIENTED_EDGE ( 'NONE', *, *, #9254, .T. ) ;
#766 = CARTESIAN_POINT ( 'NONE',  ( -62.49999999999998579, 11.16666666666666607, 2.366025403784441483 ) ) ;
#767 = VERTEX_POINT ( 'NONE', #4360 ) ;
#768 = CARTESIAN_POINT ( 'NONE',  ( -60.99999999999998579, 8.520833333333333925, 0.9226497308103762673 ) ) ;
#769 = CARTESIAN_POINT ( 'NONE',  ( -62.99999999999998579, 15.85416666666666607, 0.9226497308103756012 ) ) ;
#770 = CIRCLE ( 'NONE', #9120, 1.000000000000000000 ) ;
#771 = EDGE_CURVE ( 'NONE', #3276, #292, #2717, .T. ) ;
#772 = EDGE_CURVE ( 'NONE', #7557, #5975, #6044, .T. ) ;
#773 = CARTESIAN_POINT ( 'NONE',  ( -61.13531646874998415, 13.61979166632526983, 1.999225269531026417 ) ) ;
#774 = CARTESIAN_POINT ( 'NONE',  ( 0.6000000000000000888, 0.000000000000000000, 0.000000000000000000 ) ) ;
#775 = ORIENTED_EDGE ( 'NONE', *, *, #4849, .F. ) ;
#776 = CARTESIAN_POINT ( 'NONE',  ( -61.49999999999998579, 11.01041666598386826, 0.6339745962155628467 ) ) ;
#777 = ORIENTED_EDGE ( 'NONE', *, *, #2224, .F. ) ;
#778 = CARTESIAN_POINT ( 'NONE',  ( -61.99999999999998579, 14.28124999931720218, 0.5000000000000013323 ) ) ;
#779 = CARTESIAN_POINT ( 'NONE',  ( -61.13531646874998415, 14.55729166632526628, 1.999225269531026417 ) ) ;
#780 = DIRECTION ( 'NONE',  ( -1.000000000000000000, 0.000000000000000000, 0.000000000000000000 ) ) ;
#781 = DIRECTION ( 'NONE',  ( 1.000000000000000000, -0.000000000000000000, -0.000000000000000000 ) ) ;
#782 = DIRECTION ( 'NONE',  ( 1.000000000000000000, 0.000000000000000000, 0.000000000000000000 ) ) ;
#783 = CARTESIAN_POINT ( 'NONE',  ( -61.99999999999999289, 12.70312499965860198, 0.5015494609379544944 ) ) ;
#784 = CARTESIAN_POINT ( 'NONE',  ( -62.86468353124998032, 14.99479166632526805, 1.000774730468978246 ) ) ;
#785 = DIRECTION ( 'NONE',  ( 3.965082230804130220E-16, -1.000000000000000000, -0.000000000000000000 ) ) ;
#786 = DIRECTION ( 'NONE',  ( 1.110223024625156540E-15, -1.000000000000000000, -0.000000000000000000 ) ) ;
#787 = CARTESIAN_POINT ( 'NONE',  ( -61.13531646874998415, 8.911458332991934128, 1.000774730468978468 ) ) ;
#788 = FACE_OUTER_BOUND ( 'NONE', #1381, .T. ) ;
#789 = ORIENTED_EDGE ( 'NONE', *, *, #3107, .F. ) ;
#790 = FACE_OUTER_BOUND ( 'NONE', #694, .T. ) ;
#791 = CARTESIAN_POINT ( 'NONE',  ( -61.99999999999998579, 16.00000000000000000, 1.500000000000002220 ) ) ;
#792 = EDGE_CURVE ( 'NONE', #4570, #3615, #389, .T. ) ;
#793 = CARTESIAN_POINT ( 'NONE',  ( -61.56765823437498852, 14.03645833299193413, 2.248837904296538515 ) ) ;
#794 = CARTESIAN_POINT ( 'NONE',  ( -61.99999999999998579, 11.76562499965860198, 2.498450539062049724 ) ) ;
#795 = EDGE_CURVE ( 'NONE', #10821, #9418, #1827, .T. ) ;
#796 = CARTESIAN_POINT ( 'NONE',  ( -61.99999999999999289, 15.32812499965860198, 2.498450539062049724 ) ) ;
#797 = CARTESIAN_POINT ( 'NONE',  ( -61.49999999999998579, 14.42708333265053611, 2.366025403784441927 ) ) ;
#798 = ORIENTED_EDGE ( 'NONE', *, *, #2162, .T. ) ;
#799 = CARTESIAN_POINT ( 'NONE',  ( -61.99999999999998579, 13.43749999999999822, 2.654700538379254571 ) ) ;
#800 = CARTESIAN_POINT ( 'NONE',  ( -62.86468353124999453, 8.265624999658601979, 1.500000000000002220 ) ) ;
#801 = EDGE_CURVE ( 'NONE', #5222, #6754, #4636, .T. ) ;
#802 = CARTESIAN_POINT ( 'NONE',  ( -60.99999999999998579, 12.94791666598387003, 2.077350269189628840 ) ) ;
#803 = ORIENTED_EDGE ( 'NONE', *, *, #6363, .T. ) ;
#804 = CARTESIAN_POINT ( 'NONE',  ( -61.99999999999998579, 9.437499999999998224, 2.500000000000002665 ) ) ;
#805 =( BOUNDED_CURVE ( )  B_SPLINE_CURVE ( 2, ( #6919, #4287, #1801, #9519, #7697, #5285, #9408, #246, #76 ),
 .UNSPECIFIED., .F., .T. ) 
 B_SPLINE_CURVE_WITH_KNOTS ( ( 3, 2, 2, 2, 3 ),
 ( 0.2109375000000000000, 0.2135416666666666574, 0.2187500000000000000, 0.2239583333333333426, 0.2265625000000000000 ),
 .UNSPECIFIED. ) 
 CURVE ( )  GEOMETRIC_REPRESENTATION_ITEM ( )  RATIONAL_B_SPLINE_CURVE ( ( 0.9330127018922194093, 0.9330127018922194093, 1.000000000000000000, 0.8660254037844387076, 1.000000000000000000, 0.8660254037844387076, 1.000000000000000000, 0.9330127018922194093, 0.9330127018922194093 ) ) 
 REPRESENTATION_ITEM ( '' )  );
#806 = CARTESIAN_POINT ( 'NONE',  ( -61.13531646874998415, 14.07812499965860198, 1.500000000000002220 ) ) ;
#807 = ORIENTED_EDGE ( 'NONE', *, *, #3016, .T. ) ;
#808 = LINE ( 'NONE', #4293, #610 ) ;
#809 = CARTESIAN_POINT ( 'NONE',  ( -62.43234176562498305, 12.72395833299193413, 0.7511620957034662593 ) ) ;
#810 = CYLINDRICAL_SURFACE ( 'NONE', #2113, 0.9999999999999981126 ) ;
#811 = EDGE_CURVE ( 'NONE', #6260, #5909, #3801, .T. ) ;
#812 = ORIENTED_EDGE ( 'NONE', *, *, #91, .F. ) ;
#813 = CARTESIAN_POINT ( 'NONE',  ( 0.000000000000000000, 0.2499999999999982792, 1.312875263449799323 ) ) ;
#814 = EDGE_LOOP ( 'NONE', ( #8407, #1313, #7773, #3216 ) ) ;
#815 = CARTESIAN_POINT ( 'NONE',  ( -61.49999999999998579, 14.70833333333333393, 2.366025403784441927 ) ) ;
#816 = ORIENTED_EDGE ( 'NONE', *, *, #555, .F. ) ;
#817 = CARTESIAN_POINT ( 'NONE',  ( -60.99999999999998579, 11.52083333333333393, 0.9226497308103762673 ) ) ;
#818 = ORIENTED_EDGE ( 'NONE', *, *, #2165, .F. ) ;
#819 = CARTESIAN_POINT ( 'NONE',  ( -61.13531646874998415, 8.661458332991935904, 1.000774730468978468 ) ) ;
#820 = DIRECTION ( 'NONE',  ( -0.000000000000000000, -1.000000000000000000, -0.000000000000000000 ) ) ;
#821 = EDGE_CURVE ( 'NONE', #7309, #7701, #10603, .T. ) ;
#822 = CARTESIAN_POINT ( 'NONE',  ( -61.13531646874998415, 13.39062499965860020, 1.500000000000002220 ) ) ;
#823 = CARTESIAN_POINT ( 'NONE',  ( -61.73205080756885366, 8.270085449632572860, 0.5000000000000027756 ) ) ;
#824 = ORIENTED_EDGE ( 'NONE', *, *, #8252, .F. ) ;
#825 = DIRECTION ( 'NONE',  ( -0.000000000000000000, 0.000000000000000000, 1.000000000000000000 ) ) ;
#826 = EDGE_CURVE ( 'NONE', #1612, #7049, #10099, .T. ) ;
#827 = VERTEX_POINT ( 'NONE', #6776 ) ;
#828 = CARTESIAN_POINT ( 'NONE',  ( -60.99999999999998579, 12.75000000000000178, 1.500000000000002220 ) ) ;
#829 = CARTESIAN_POINT ( 'NONE',  ( -61.99999999999998579, 15.39062499965860198, 0.5015494609379544944 ) ) ;
#830 = CARTESIAN_POINT ( 'NONE',  ( -60.99999999999998579, 16.00000000000000000, 1.500000000000002220 ) ) ;
#831 = DIRECTION ( 'NONE',  ( -0.000000000000000000, 1.000000000000000000, 0.000000000000000000 ) ) ;
#832 = CARTESIAN_POINT ( 'NONE',  ( -62.43234176562499016, 13.05729166632526805, 2.248837904296538071 ) ) ;
#833 = CARTESIAN_POINT ( 'NONE',  ( -61.56765823437498852, 15.34895833299193590, 2.248837904296538515 ) ) ;
#834 = CARTESIAN_POINT ( 'NONE',  ( -61.99999999999998579, 16.00000000000000000, 1.500000000000002220 ) ) ;
#835 = CARTESIAN_POINT ( 'NONE',  ( -61.99999999999998579, 8.812500000000000000, 0.5000000000000013323 ) ) ;
#836 = VECTOR ( 'NONE', #5537, 1000.000000000000000 ) ;
#837 = CARTESIAN_POINT ( 'NONE',  ( -62.86468353124998742, 9.536458332991935904, 1.999225269531025972 ) ) ;
#838 = DIRECTION ( 'NONE',  ( 0.000000000000000000, 0.000000000000000000, -1.000000000000000000 ) ) ;
#839 = EDGE_LOOP ( 'NONE', ( #2453, #10131 ) ) ;
#840 = DIRECTION ( 'NONE',  ( 1.000000000000000000, 0.000000000000000000, 0.000000000000000000 ) ) ;
#841 = CARTESIAN_POINT ( 'NONE',  ( -62.99999999999998579, 12.64583333333333393, 2.077350269189627952 ) ) ;
#842 = CARTESIAN_POINT ( 'NONE',  ( -61.56765823437498142, 15.11979166632526805, 0.7511620957034663704 ) ) ;
#843 = CARTESIAN_POINT ( 'NONE',  ( -61.56765823437498142, 11.61979166632526805, 0.7511620957034663704 ) ) ;
#844 = VECTOR ( 'NONE', #7783, 1000.000000000000000 ) ;
#845 = CARTESIAN_POINT ( 'NONE',  ( -62.43234176562498305, 15.47395833299193590, 0.7511620957034662593 ) ) ;
#846 = DIRECTION ( 'NONE',  ( -0.000000000000000000, -0.000000000000000000, -1.000000000000000000 ) ) ;
#847 = VERTEX_POINT ( 'NONE', #1713 ) ;
#848 = CARTESIAN_POINT ( 'NONE',  ( -60.99999999999998579, 14.47916666666666607, 2.077350269189628840 ) ) ;
#849 = CARTESIAN_POINT ( 'NONE',  ( -61.13531646874998415, 8.140624999658601979, 1.500000000000002220 ) ) ;
#850 =( NAMED_UNIT ( * ) PLANE_ANGLE_UNIT ( ) SI_UNIT ( $, .RADIAN. ) );
#851 = EDGE_CURVE ( 'NONE', #8859, #6858, #8491, .T. ) ;
#852 = CARTESIAN_POINT ( 'NONE',  ( -60.99999999999998579, 12.96874999931720396, 1.500000000000002220 ) ) ;
#853 = CARTESIAN_POINT ( 'NONE',  ( 0.000000000000000000, 2.500000000000000000, 3.000000000000000000 ) ) ;
#854 = PRESENTATION_LAYER_ASSIGNMENT (  '', '', ( #5815 ) ) ;
#855 = EDGE_CURVE ( 'NONE', #8551, #10821, #6065, .T. ) ;
#856 = VECTOR ( 'NONE', #4422, 1000.000000000000000 ) ;
#857 = CARTESIAN_POINT ( 'NONE',  ( -62.86468353124998032, 12.18229166632526628, 1.000774730468978024 ) ) ;
#858 = ORIENTED_EDGE ( 'NONE', *, *, #4449, .T. ) ;
#859 = DIRECTION ( 'NONE',  ( -0.000000000000000000, -0.000000000000000000, -1.000000000000000000 ) ) ;
#860 = CARTESIAN_POINT ( 'NONE',  ( -61.13531646874998415, 13.41145833299193235, 1.000774730468978468 ) ) ;
#861 = CARTESIAN_POINT ( 'NONE',  ( -61.06765823437498852, 16.03906249982930277, 1.500000000000002220 ) ) ;
#862 = VECTOR ( 'NONE', #785, 1000.000000000000000 ) ;
#863 = ORIENTED_EDGE ( 'NONE', *, *, #9461, .F. ) ;
#864 = CARTESIAN_POINT ( 'NONE',  ( -61.99999999999998579, 9.281249999317202182, 0.5000000000000013323 ) ) ;
#865 = ORIENTED_EDGE ( 'NONE', *, *, #10184, .F. ) ;
#866 = CARTESIAN_POINT ( 'NONE',  ( -49.99999999999998579, -14.00000000000001243, 3.000000000000000000 ) ) ;
#867 = VECTOR ( 'NONE', #10902, 1000.000000000000000 ) ;
#868 = ADVANCED_FACE ( 'NONE', ( #4599 ), #2169, .T. ) ;
#869 = VERTEX_POINT ( 'NONE', #5544 ) ;
#870 = ORIENTED_EDGE ( 'NONE', *, *, #9959, .T. ) ;
#871 = CARTESIAN_POINT ( 'NONE',  ( -62.43234176562499016, 8.557291666325268054, 2.248837904296538071 ) ) ;
#872 = CARTESIAN_POINT ( 'NONE',  ( -60.99999999999998579, 14.22916666666666785, 2.077350269189628840 ) ) ;
#873 = VECTOR ( 'NONE', #2385, 1000.000000000000000 ) ;
#874 = CARTESIAN_POINT ( 'NONE',  ( -62.43234176562499016, 13.55729166632526805, 2.248837904296538071 ) ) ;
#875 = PRESENTATION_LAYER_ASSIGNMENT (  '', '', ( #4072 ) ) ;
#876 = CARTESIAN_POINT ( 'NONE',  ( -62.99999999999998579, 12.84374999931720396, 1.500000000000001998 ) ) ;
#877 = EDGE_LOOP ( 'NONE', ( #7744, #7640, #7709, #8703, #6978 ) ) ;
#878 = CARTESIAN_POINT ( 'NONE',  ( -61.49999999999998579, 10.92708333265053611, 2.366025403784441927 ) ) ;
#879 = AXIS2_PLACEMENT_3D ( 'NONE', #2223, #3056, #5655 ) ;
#880 = ORIENTED_EDGE ( 'NONE', *, *, #964, .F. ) ;
#881 = CARTESIAN_POINT ( 'NONE',  ( -62.26794919243111082, 11.54241454900183150, 0.5000000000000013323 ) ) ;
#882 = CARTESIAN_POINT ( 'NONE',  ( -61.99999999999998579, 14.64062499965860020, 0.5015494609379544944 ) ) ;
#883 = DIRECTION ( 'NONE',  ( -0.000000000000000000, -0.000000000000000000, 1.000000000000000000 ) ) ;
#884 = CARTESIAN_POINT ( 'NONE',  ( -61.99999999999998579, 12.40624999931720218, 2.500000000000002665 ) ) ;
#885 = CARTESIAN_POINT ( 'NONE',  ( -61.73205080756886076, 10.80133545031537068, 0.5000000000000014433 ) ) ;
#886 = CARTESIAN_POINT ( 'NONE',  ( -61.56765823437498852, 12.34895833299193413, 2.248837904296538515 ) ) ;
#887 = CARTESIAN_POINT ( 'NONE',  ( -62.43234176562498305, 8.661458332991934128, 0.7511620957034662593 ) ) ;
#888 = LINE ( 'NONE', #4120, #699 ) ;
#889 = CARTESIAN_POINT ( 'NONE',  ( -62.43234176562498305, 8.973958332991934128, 0.7511620957034662593 ) ) ;
#890 = CARTESIAN_POINT ( 'NONE',  ( -61.73205080756886076, 15.66741454900183506, 2.500000000000003109 ) ) ;
#891 = ORIENTED_EDGE ( 'NONE', *, *, #2292, .T. ) ;
#892 = CARTESIAN_POINT ( 'NONE',  ( -114.9999999999999289, -7.999999999999998224, 0.000000000000000000 ) ) ;
#893 = CARTESIAN_POINT ( 'NONE',  ( -61.99999999999998579, 16.00000000000000000, 1.500000000000002220 ) ) ;
#894 = CARTESIAN_POINT ( 'NONE',  ( -62.86468353124999453, 15.45312499965860020, 1.500000000000002220 ) ) ;
#895 = CARTESIAN_POINT ( 'NONE',  ( -61.13531646874998415, 11.84895833299193413, 1.000774730468978468 ) ) ;
#896 = CARTESIAN_POINT ( 'NONE',  ( -62.86468353124998032, 15.24479166632526805, 1.000774730468978024 ) ) ;
#897 =( LENGTH_UNIT ( ) NAMED_UNIT ( * ) SI_UNIT ( .MILLI., .METRE. ) );
#898 = ORIENTED_EDGE ( 'NONE', *, *, #8338, .F. ) ;
#899 = CARTESIAN_POINT ( 'NONE',  ( -62.99999999999998579, 14.62500000000000000, 1.500000000000001998 ) ) ;
#900 = CARTESIAN_POINT ( 'NONE',  ( -61.99999999999999289, 8.453124999658601979, 0.5015494609379544944 ) ) ;
#901 = EDGE_CURVE ( 'NONE', #10100, #8518, #3651, .T. ) ;
#902 = CARTESIAN_POINT ( 'NONE',  ( -61.49999999999998579, 13.01041666598386826, 0.6339745962155628467 ) ) ;
#903 = DIRECTION ( 'NONE',  ( -1.000000000000000000, 0.000000000000000000, 0.000000000000000000 ) ) ;
#904 = CARTESIAN_POINT ( 'NONE',  ( -61.99999999999998579, 11.31250000000000000, 0.5000000000000013323 ) ) ;
#905 = AXIS2_PLACEMENT_3D ( 'NONE', #10068, #7575, #3243 ) ;
#906 = CARTESIAN_POINT ( 'NONE',  ( -62.86468353124999453, 10.97395833299193413, 1.999225269531025750 ) ) ;
#907 = SURFACE_STYLE_FILL_AREA ( #10966 ) ;
#908 = CARTESIAN_POINT ( 'NONE',  ( -43.00000000000000711, -14.00000000000000888, 5.000000000000000000 ) ) ;
#909 = ORIENTED_EDGE ( 'NONE', *, *, #963, .T. ) ;
#910 = CARTESIAN_POINT ( 'NONE',  ( -62.99999999999998579, 12.89583333333333037, 2.077350269189627952 ) ) ;
#911 = ADVANCED_FACE ( 'NONE', ( #5426 ), #6787, .F. ) ;
#912 = CARTESIAN_POINT ( 'NONE',  ( -61.56765823437498142, 13.18229166632526805, 0.7511620957034663704 ) ) ;
#913 = CARTESIAN_POINT ( 'NONE',  ( -61.99999999999998579, 16.00000000000000000, 2.500000000000000444 ) ) ;
#914 = AXIS2_PLACEMENT_3D ( 'NONE', #7457, #10834, #3218 ) ;
#915 = CARTESIAN_POINT ( 'NONE',  ( -62.49999999999998579, 9.885416665983870033, 2.366025403784441483 ) ) ;
#916 = ORIENTED_EDGE ( 'NONE', *, *, #2745, .F. ) ;
#917 = LINE ( 'NONE', #10976, #7086 ) ;
#918 = VERTEX_POINT ( 'NONE', #9716 ) ;
#919 = CARTESIAN_POINT ( 'NONE',  ( -60.99999999999998579, 14.72916666666666607, 2.077350269189628840 ) ) ;
#920 = CARTESIAN_POINT ( 'NONE',  ( -62.43234176562498305, 10.66145833299193413, 0.7511620957034662593 ) ) ;
#921 = AXIS2_PLACEMENT_3D ( 'NONE', #4939, #10835, #4055 ) ;
#922 =( NAMED_UNIT ( * ) SI_UNIT ( $, .STERADIAN. ) SOLID_ANGLE_UNIT ( ) );
#923 = ORIENTED_EDGE ( 'NONE', *, *, #6486, .F. ) ;
#924 = ADVANCED_FACE ( 'NONE', ( #6277 ), #5310, .T. ) ;
#925 = CARTESIAN_POINT ( 'NONE',  ( -61.99999999999998579, 9.453124999658600203, 0.5015494609379544944 ) ) ;
#926 = CARTESIAN_POINT ( 'NONE',  ( -62.99999999999998579, 13.82291666598387003, 0.9226497308103756012 ) ) ;
#927 = CIRCLE ( 'NONE', #2364, 1.928074011315806136 ) ;
#928 = EDGE_CURVE ( 'NONE', #847, #6070, #402, .T. ) ;
#929 = CARTESIAN_POINT ( 'NONE',  ( -62.86468353124998032, 13.49479166632526805, 1.000774730468978246 ) ) ;
#930 = VERTEX_POINT ( 'NONE', #6996 ) ;
#931 = FACE_OUTER_BOUND ( 'NONE', #8908, .T. ) ;
#932 = PRODUCT_DEFINITION ( 'UNKNOWN', '', #1061, #2065 ) ;
#933 = ORIENTED_EDGE ( 'NONE', *, *, #3473, .F. ) ;
#934 = VECTOR ( 'NONE', #6411, 1000.000000000000000 ) ;
#935 = CARTESIAN_POINT ( 'NONE',  ( -62.49999999999998579, 11.63541666598387003, 2.366025403784441483 ) ) ;
#936 = CARTESIAN_POINT ( 'NONE',  ( -61.56765823437498852, 14.53645833299193413, 2.248837904296538515 ) ) ;
#937 = DIRECTION ( 'NONE',  ( -0.000000000000000000, -0.000000000000000000, -1.000000000000000000 ) ) ;
#938 = CARTESIAN_POINT ( 'NONE',  ( -60.99999999999998579, 12.47916666666666785, 2.077350269189628840 ) ) ;
#939 = PLANE ( 'NONE',  #2806 ) ;
#940 = CARTESIAN_POINT ( 'NONE',  ( -61.99999999999999289, 14.07812499965860020, 2.498450539062049724 ) ) ;
#941 = CARTESIAN_POINT ( 'NONE',  ( -62.86468353124999453, 8.453124999658601979, 1.500000000000002220 ) ) ;
#942 = CARTESIAN_POINT ( 'NONE',  ( -61.99999999999998579, 16.00000000000000000, 1.500000000000002220 ) ) ;
#943 = EDGE_CURVE ( 'NONE', #5113, #386, #9778, .T. ) ;
#944 = CYLINDRICAL_SURFACE ( 'NONE', #4058, 1.099999999999989875 ) ;
#945 = CARTESIAN_POINT ( 'NONE',  ( -62.86468353124998742, 9.286458332991934128, 1.999225269531025972 ) ) ;
#946 = CARTESIAN_POINT ( 'NONE',  ( -1.470152734901925752E-14, 0.2499999999999982792, -1.453737367178236983 ) ) ;
#947 = VERTEX_POINT ( 'NONE', #1277 ) ;
#948 = CARTESIAN_POINT ( 'NONE',  ( 195.0000000000000000, -2.500000000000000000, 4.000000000000000000 ) ) ;
#949 = CARTESIAN_POINT ( 'NONE',  ( 195.0000000000000000, -2.500000000000000000, 2.000000000000000000 ) ) ;
#950 = CARTESIAN_POINT ( 'NONE',  ( -61.56765823437498852, 15.78645833299193590, 2.248837904296538515 ) ) ;
#951 = CARTESIAN_POINT ( 'NONE',  ( -61.13531646874998415, 10.55729166632526805, 1.999225269531026417 ) ) ;
#952 = CARTESIAN_POINT ( 'NONE',  ( -62.43234176562499016, 9.494791666325268054, 2.248837904296538071 ) ) ;
#953 = ORIENTED_EDGE ( 'NONE', *, *, #8718, .T. ) ;
#954 = CARTESIAN_POINT ( 'NONE',  ( -62.99999999999998579, 14.85416666666666607, 0.9226497308103756012 ) ) ;
#955 = CARTESIAN_POINT ( 'NONE',  ( -61.99999999999999289, 10.70312499965860198, 0.5015494609379544944 ) ) ;
#956 = DIRECTION ( 'NONE',  ( 1.000000000000000000, 0.000000000000000000, 0.000000000000000000 ) ) ;
#957 = CARTESIAN_POINT ( 'NONE',  ( -61.99999999999998579, 12.90624999931720396, 2.654700538379254571 ) ) ;
#958 = CARTESIAN_POINT ( 'NONE',  ( -62.49999999999998579, 13.16666666666666607, 2.366025403784441483 ) ) ;
#959 =( BOUNDED_CURVE ( )  B_SPLINE_CURVE ( 2, ( #8529, #966, #8702, #10294, #191, #3522, #4402, #10355, #8759 ),
 .UNSPECIFIED., .F., .T. ) 
 B_SPLINE_CURVE_WITH_KNOTS ( ( 3, 2, 2, 2, 3 ),
 ( 0.6171875000000000000, 0.6197916666666666297, 0.6250000000000000000, 0.6302083333333333703, 0.6328125000000000000 ),
 .UNSPECIFIED. ) 
 CURVE ( )  GEOMETRIC_REPRESENTATION_ITEM ( )  RATIONAL_B_SPLINE_CURVE ( ( 0.9330127018922194093, 0.9330127018922194093, 1.000000000000000000, 0.8660254037844387076, 1.000000000000000000, 0.8660254037844387076, 1.000000000000000000, 0.9330127018922194093, 0.9330127018922194093 ) ) 
 REPRESENTATION_ITEM ( '' )  );
#960 = EDGE_CURVE ( 'NONE', #5520, #211, #7167, .T. ) ;
#961 = PLANE ( 'NONE',  #222 ) ;
#962 = CARTESIAN_POINT ( 'NONE',  ( -61.99999999999999289, 11.89062499965860553, 0.5015494609379544944 ) ) ;
#963 = EDGE_CURVE ( 'NONE', #2018, #6810, #1525, .T. ) ;
#964 = EDGE_CURVE ( 'NONE', #4466, #8509, #4114, .T. ) ;
#965 = DIRECTION ( 'NONE',  ( -0.000000000000000000, -1.000000000000000000, -0.000000000000000000 ) ) ;
#966 = CARTESIAN_POINT ( 'NONE',  ( -61.73205080756886076, 12.94866454968462932, 2.500000000000003109 ) ) ;
#967 = EDGE_LOOP ( 'NONE', ( #3059, #1127, #10448, #2159 ) ) ;
#968 = CARTESIAN_POINT ( 'NONE',  ( -46.99999999999998579, -15.00000000000001066, 0.000000000000000000 ) ) ;
#969 = CARTESIAN_POINT ( 'NONE',  ( -61.56765823437498852, 12.34895833299193413, 2.248837904296538515 ) ) ;
#970 = SURFACE_STYLE_USAGE ( .BOTH. , #1755 ) ;
#971 = CARTESIAN_POINT ( 'NONE',  ( -62.26794919243111082, 13.82366454968463110, 0.5000000000000013323 ) ) ;
#972 = CARTESIAN_POINT ( 'NONE',  ( -62.99999999999998579, 9.843749999317202182, 1.500000000000001998 ) ) ;
#973 = EDGE_LOOP ( 'NONE', ( #9490, #7582 ) ) ;
#974 = CARTESIAN_POINT ( 'NONE',  ( -61.99999999999998579, 14.99999999999998579, 0.5000000000000013323 ) ) ;
#975 = CARTESIAN_POINT ( 'NONE',  ( -61.99999999999998579, 16.00000000000000000, 1.500000000000002220 ) ) ;
#976 = CARTESIAN_POINT ( 'NONE',  ( -62.43234176562498305, 11.16145833299193590, 0.7511620957034662593 ) ) ;
#977 = ORIENTED_EDGE ( 'NONE', *, *, #9014, .T. ) ;
#978 = CARTESIAN_POINT ( 'NONE',  ( -62.86468353124999453, 9.265624999658600203, 1.500000000000002220 ) ) ;
#979 = DIRECTION ( 'NONE',  ( 0.000000000000000000, -0.000000000000000000, -1.000000000000000000 ) ) ;
#980 = ADVANCED_FACE ( 'NONE', ( #3711 ), #7111, .F. ) ;
#981 = CARTESIAN_POINT ( 'NONE',  ( -62.86468353124998032, 14.99479166632526805, 1.000774730468978246 ) ) ;
#982 = CARTESIAN_POINT ( 'NONE',  ( -62.99999999999998579, 9.343749999317202182, 1.500000000000001998 ) ) ;
#983 = ORIENTED_EDGE ( 'NONE', *, *, #2088, .F. ) ;
#984 = LINE ( 'NONE', #3485, #6922 ) ;
#985 = EDGE_CURVE ( 'NONE', #4938, #4740, #10490, .T. ) ;
#986 = EDGE_LOOP ( 'NONE', ( #1772, #5582, #9425, #3019 ) ) ;
#987 = CARTESIAN_POINT ( 'NONE',  ( -61.99999999999998579, 13.15624999931720218, 2.500000000000002665 ) ) ;
#988 = CARTESIAN_POINT ( 'NONE',  ( -60.99999999999998579, 8.250000000000000000, 1.500000000000002220 ) ) ;
#989 = CARTESIAN_POINT ( 'NONE',  ( -31.99999999999998579, -14.00000000000000888, -0.9999999999999947820 ) ) ;
#990 = CARTESIAN_POINT ( 'NONE',  ( -60.99999999999998579, 12.52083333333333215, 0.9226497308103762673 ) ) ;
#991 = LINE ( 'NONE', #10159, #844 ) ;
#992 = CARTESIAN_POINT ( 'NONE',  ( -61.13531646874997705, 14.11979166632526805, 1.999225269531026417 ) ) ;
#993 = CARTESIAN_POINT ( 'NONE',  ( -61.99999999999998579, 8.640624999658601979, 0.5015494609379544944 ) ) ;
#994 = DIRECTION ( 'NONE',  ( 1.000000000000000000, 0.000000000000000000, 0.000000000000000000 ) ) ;
#995 = FACE_OUTER_BOUND ( 'NONE', #3796, .T. ) ;
#996 = CARTESIAN_POINT ( 'NONE',  ( -62.86468353124999453, 9.765624999658601979, 1.500000000000002220 ) ) ;
#997 = CARTESIAN_POINT ( 'NONE',  ( 1.299999999999999156, 0.000000000000000000, 1.000000000000000000 ) ) ;
#998 = ORIENTED_EDGE ( 'NONE', *, *, #7274, .T. ) ;
#999 = DIRECTION ( 'NONE',  ( -1.000000000000000000, 0.000000000000000000, -0.000000000000000000 ) ) ;
#1000 = FACE_OUTER_BOUND ( 'NONE', #6370, .T. ) ;
#1001 = APPLICATION_CONTEXT ( 'automotive_design' ) ;
#1002 = CARTESIAN_POINT ( 'NONE',  ( -61.56765823437498852, 16.03645833299193768, 2.248837904296538515 ) ) ;
#1003 = EDGE_CURVE ( 'NONE', #6871, #7309, #7220, .T. ) ;
#1004 = CARTESIAN_POINT ( 'NONE',  ( -62.86468353124999453, 11.45312499965860020, 1.500000000000002220 ) ) ;
#1005 = CARTESIAN_POINT ( 'NONE',  ( -61.56765823437498852, 8.286458332991934128, 2.248837904296538515 ) ) ;
#1006 = ORIENTED_EDGE ( 'NONE', *, *, #5250, .T. ) ;
#1007 = CARTESIAN_POINT ( 'NONE',  ( -61.49999999999998579, 15.29166666666666607, 0.6339745962155628467 ) ) ;
#1008 = CARTESIAN_POINT ( 'NONE',  ( -61.99999999999999289, 10.20312499965860198, 0.5015494609379544944 ) ) ;
#1009 = AXIS2_PLACEMENT_3D ( 'NONE', #2485, #7596, #1705 ) ;
#1010 =( NAMED_UNIT ( * ) PLANE_ANGLE_UNIT ( ) SI_UNIT ( $, .RADIAN. ) );
#1011 = CARTESIAN_POINT ( 'NONE',  ( -62.99999999999998579, 13.11458333265053433, 2.077350269189627952 ) ) ;
#1012 = CARTESIAN_POINT ( 'NONE',  ( -62.26794919243111082, 13.17633545031536890, 2.500000000000003109 ) ) ;
#1013 = ORIENTED_EDGE ( 'NONE', *, *, #2371, .T. ) ;
#1014 = DIRECTION ( 'NONE',  ( 0.000000000000000000, 0.000000000000000000, -1.000000000000000000 ) ) ;
#1015 = AXIS2_PLACEMENT_3D ( 'NONE', #7511, #8290, #2342 ) ;
#1016 = CARTESIAN_POINT ( 'NONE',  ( -61.13531646874998415, 11.32812499965860020, 1.500000000000002220 ) ) ;
#1017 = CYLINDRICAL_SURFACE ( 'NONE', #3505, 1.099999999999989875 ) ;
#1018 = DIRECTION ( 'NONE',  ( 0.8660254037844418162, 0.4999999999999947264, -0.000000000000000000 ) ) ;
#1019 = ORIENTED_EDGE ( 'NONE', *, *, #10039, .F. ) ;
#1020 = CARTESIAN_POINT ( 'NONE',  ( -62.49999999999998579, 11.33333333333333393, 0.6339745962155627357 ) ) ;
#1021 = DIRECTION ( 'NONE',  ( 1.000000000000000000, 0.000000000000000000, 0.000000000000000000 ) ) ;
#1022 = CARTESIAN_POINT ( 'NONE',  ( -61.56765823437498142, 14.18229166632526805, 0.7511620957034663704 ) ) ;
#1023 =( BOUNDED_CURVE ( )  B_SPLINE_CURVE ( 2, ( #1890, #6286, #10383, #10558, #1287, #9611, #1048, #2843, #8840 ),
 .UNSPECIFIED., .F., .F. ) 
 B_SPLINE_CURVE_WITH_KNOTS ( ( 3, 2, 2, 2, 3 ),
 ( 0.3046874999999999445, 0.3072916666666666852, 0.3125000000000000000, 0.3177083333333333148, 0.3203125000000000000 ),
 .UNSPECIFIED. ) 
 CURVE ( )  GEOMETRIC_REPRESENTATION_ITEM ( )  RATIONAL_B_SPLINE_CURVE ( ( 0.9330127018922192983, 0.9330127018922178550, 1.000000000000000000, 0.8660254037844387076, 1.000000000000000000, 0.8660254037844387076, 1.000000000000000000, 0.9330127018922194093, 0.9330127018922194093 ) ) 
 REPRESENTATION_ITEM ( '' )  );
#1024 = FACE_OUTER_BOUND ( 'NONE', #3434, .T. ) ;
#1025 = AXIS2_PLACEMENT_3D ( 'NONE', #9855, #4728, #3739 ) ;
#1026 = CARTESIAN_POINT ( 'NONE',  ( -60.99999999999998579, 8.989583332650536107, 0.9226497308103762673 ) ) ;
#1027 = EDGE_LOOP ( 'NONE', ( #8715, #10682 ) ) ;
#1028 = CARTESIAN_POINT ( 'NONE',  ( -134.9999999999999147, 8.000000000000000000, 0.000000000000000000 ) ) ;
#1029 = AXIS2_PLACEMENT_3D ( 'NONE', #1383, #4866, #8270 ) ;
#1030 = CARTESIAN_POINT ( 'NONE',  ( -109.9999999999999574, 14.99999999999998579, 83.15773105863907233 ) ) ;
#1031 = CARTESIAN_POINT ( 'NONE',  ( -62.86468353124999453, 10.95312499965860020, 1.500000000000002220 ) ) ;
#1032 = AXIS2_PLACEMENT_3D ( 'NONE', #4772, #3269, #6667 ) ;
#1033 = ORIENTED_EDGE ( 'NONE', *, *, #9359, .T. ) ;
#1034 = CARTESIAN_POINT ( 'NONE',  ( -62.43234176562498305, 9.723958332991934128, 0.7511620957034662593 ) ) ;
#1035 = CARTESIAN_POINT ( 'NONE',  ( -62.26794919243111082, 15.54241454900183506, 0.5000000000000013323 ) ) ;
#1036 = AXIS2_PLACEMENT_3D ( 'NONE', #5926, #711, #4093 ) ;
#1037 = CARTESIAN_POINT ( 'NONE',  ( -61.56765823437498852, 15.09895833299193590, 2.248837904296538515 ) ) ;
#1038 = CARTESIAN_POINT ( 'NONE',  ( -61.73205080756886076, 13.30133545031536890, 0.5000000000000014433 ) ) ;
#1039 = ORIENTED_EDGE ( 'NONE', *, *, #2073, .T. ) ;
#1040 = CARTESIAN_POINT ( 'NONE',  ( -61.99999999999998579, 15.31250000000000000, 0.5000000000000013323 ) ) ;
#1041 = COLOUR_RGB ( '',0.8941176470588234615, 0.8941176470588234615, 0.8941176470588234615 ) ;
#1042 = ORIENTED_EDGE ( 'NONE', *, *, #6230, .T. ) ;
#1043 = CARTESIAN_POINT ( 'NONE',  ( -49.99999999999998579, 14.99999999999998579, 5.000000000000004441 ) ) ;
#1044 = CARTESIAN_POINT ( 'NONE',  ( -61.99999999999998579, 15.89062499965860198, 0.5015494609379544944 ) ) ;
#1045 = VECTOR ( 'NONE', #1236, 1000.000000000000000 ) ;
#1046 = CARTESIAN_POINT ( 'NONE',  ( -61.99999999999998579, 16.00000000000000000, 1.500000000000002220 ) ) ;
#1047 = CARTESIAN_POINT ( 'NONE',  ( -61.49999999999998579, 12.42708333265053611, 2.366025403784441927 ) ) ;
#1048 = CARTESIAN_POINT ( 'NONE',  ( -61.49999999999998579, 10.76041666598386826, 0.6339745962155628467 ) ) ;
#1049 = CARTESIAN_POINT ( 'NONE',  ( -61.13531646874997705, 14.41145833299193413, 1.000774730468978468 ) ) ;
#1050 = CARTESIAN_POINT ( 'NONE',  ( -61.99999999999998579, 9.140624999658601979, 0.5015494609379544944 ) ) ;
#1051 = ADVANCED_FACE ( 'NONE', ( #3001 ), #6391, .F. ) ;
#1052 = AXIS2_PLACEMENT_3D ( 'NONE', #356, #4512, #6421 ) ;
#1053 = DIRECTION ( 'NONE',  ( -1.000000000000000000, 0.000000000000000000, 0.000000000000000000 ) ) ;
#1054 = CARTESIAN_POINT ( 'NONE',  ( -62.26794919243111082, 9.573664549684629321, 0.4999999999999998890 ) ) ;
#1055 = CARTESIAN_POINT ( 'NONE',  ( -62.86468353124998032, 9.994791666325268054, 1.000774730468978246 ) ) ;
#1056 = CARTESIAN_POINT ( 'NONE',  ( -144.9999999999999432, 8.000000000000000000, 0.000000000000000000 ) ) ;
#1057 = ORIENTED_EDGE ( 'NONE', *, *, #4867, .F. ) ;
#1058 = DIRECTION ( 'NONE',  ( -0.000000000000000000, 1.000000000000000000, 1.224646799147353207E-16 ) ) ;
#1059 = DIRECTION ( 'NONE',  ( -0.000000000000000000, -1.000000000000000000, -0.000000000000000000 ) ) ;
#1060 = VECTOR ( 'NONE', #10492, 1000.000000000000000 ) ;
#1061 = PRODUCT_DEFINITION_FORMATION_WITH_SPECIFIED_SOURCE ( 'ANY', '', #5186, .NOT_KNOWN. ) ;
#1062 = CARTESIAN_POINT ( 'NONE',  ( -61.13531646874998415, 15.82812499965860198, 1.500000000000002220 ) ) ;
#1063 = CARTESIAN_POINT ( 'NONE',  ( -61.99999999999998579, 12.26562499965860198, 2.498450539062049724 ) ) ;
#1064 = CARTESIAN_POINT ( 'NONE',  ( -62.86468353124999453, 9.223958332991935904, 1.999225269531025750 ) ) ;
#1065 = DIRECTION ( 'NONE',  ( 0.000000000000000000, 1.000000000000000000, 0.000000000000000000 ) ) ;
#1066 = VERTEX_POINT ( 'NONE', #4484 ) ;
#1067 = CARTESIAN_POINT ( 'NONE',  ( -60.99999999999998579, 14.52083333333333215, 0.9226497308103762673 ) ) ;
#1068 = CARTESIAN_POINT ( 'NONE',  ( -61.13531646874997705, 9.869791666325266277, 1.999225269531026417 ) ) ;
#1069 = CARTESIAN_POINT ( 'NONE',  ( -61.13531646874998415, 14.82812499965860020, 1.500000000000002220 ) ) ;
#1070 = CARTESIAN_POINT ( 'NONE',  ( -60.99999999999998579, 14.69791666598386826, 2.077350269189628840 ) ) ;
#1071 = CARTESIAN_POINT ( 'NONE',  ( -62.99999999999998579, 13.14583333333333215, 2.077350269189627952 ) ) ;
#1072 = ORIENTED_EDGE ( 'NONE', *, *, #7222, .F. ) ;
#1073 = ADVANCED_FACE ( 'NONE', ( #5964 ), #10913, .T. ) ;
#1074 = CARTESIAN_POINT ( 'NONE',  ( -61.99999999999998579, 12.93750000000000178, 2.500000000000002665 ) ) ;
#1075 = CARTESIAN_POINT ( 'NONE',  ( -62.43234176562498305, 11.91145833299193413, 0.7511620957034662593 ) ) ;
#1076 = CARTESIAN_POINT ( 'NONE',  ( -62.43234176562498305, 9.161458332991935904, 0.7511620957034662593 ) ) ;
#1077 = CARTESIAN_POINT ( 'NONE',  ( -134.9999999999999147, 10.63932022500203267, 3.000000000000000000 ) ) ;
#1078 = ORIENTED_EDGE ( 'NONE', *, *, #5299, .T. ) ;
#1079 = CARTESIAN_POINT ( 'NONE',  ( -62.49999999999998579, 10.83333333333333393, 0.6339745962155627357 ) ) ;
#1080 = DIRECTION ( 'NONE',  ( 0.000000000000000000, 1.000000000000000000, 0.000000000000000000 ) ) ;
#1081 = CARTESIAN_POINT ( 'NONE',  ( -62.86468353124998032, 14.49479166632526805, 1.000774730468978246 ) ) ;
#1082 = FACE_OUTER_BOUND ( 'NONE', #624, .T. ) ;
#1083 = CARTESIAN_POINT ( 'NONE',  ( -60.99999999999998579, 8.739583332650536107, 0.9226497308103762673 ) ) ;
#1084 = ORIENTED_EDGE ( 'NONE', *, *, #7761, .F. ) ;
#1085 = MECHANICAL_DESIGN_GEOMETRIC_PRESENTATION_REPRESENTATION (  '', ( #8755 ), #4269 ) ;
#1086 = CARTESIAN_POINT ( 'NONE',  ( -61.49999999999998579, 14.04166666666666785, 0.6339745962155628467 ) ) ;
#1087 =( REPRESENTATION_RELATIONSHIP ('NONE','NONE', #560, #5016 ) REPRESENTATION_RELATIONSHIP_WITH_TRANSFORMATION ( #2346 )SHAPE_REPRESENTATION_RELATIONSHIP( ) );
#1088 = CARTESIAN_POINT ( 'NONE',  ( -77.99999999999998579, 0.000000000000000000, 13.00000000000000178 ) ) ;
#1089 = CARTESIAN_POINT ( 'NONE',  ( -61.13531646874998415, 11.32812499965860020, 1.500000000000002220 ) ) ;
#1090 =( NAMED_UNIT ( * ) PLANE_ANGLE_UNIT ( ) SI_UNIT ( $, .RADIAN. ) );
#1091 =( BOUNDED_CURVE ( )  B_SPLINE_CURVE ( 2, ( #4781, #2016, #7067, #9850, #10450, #2236, #5617, #2964, #2851 ),
 .UNSPECIFIED., .F., .T. ) 
 B_SPLINE_CURVE_WITH_KNOTS ( ( 3, 2, 2, 2, 3 ),
 ( 0.8984375000000000000, 0.9010416666666666297, 0.9062500000000000000, 0.9114583333333333703, 0.9140625000000000000 ),
 .UNSPECIFIED. ) 
 CURVE ( )  GEOMETRIC_REPRESENTATION_ITEM ( )  RATIONAL_B_SPLINE_CURVE ( ( 0.9330127018922194093, 0.9330127018922194093, 1.000000000000000000, 0.8660254037844387076, 1.000000000000000000, 0.8660254037844387076, 1.000000000000000000, 0.9330127018922194093, 0.9330127018922194093 ) ) 
 REPRESENTATION_ITEM ( '' )  );
#1092 = ORIENTED_EDGE ( 'NONE', *, *, #9052, .T. ) ;
#1093 = CLOSED_SHELL ( 'NONE', ( #1605, #6, #911, #5905, #8098, #4751, #1537, #8268, #4567, #7532, #4371, #5992, #8739, #7906 ) ) ;
#1094 = CARTESIAN_POINT ( 'NONE',  ( -61.13531646874998415, 9.661458332991932352, 1.000774730468978468 ) ) ;
#1095 = CARTESIAN_POINT ( 'NONE',  ( -61.99999999999998579, 15.53124999931720041, 0.5000000000000013323 ) ) ;
#1096 = MANIFOLD_SOLID_BREP ( 'Slot', #8918 ) ;
#1097 = CARTESIAN_POINT ( 'NONE',  ( -61.13531646874998415, 14.36979166632527161, 1.999225269531026417 ) ) ;
#1098 = DIRECTION ( 'NONE',  ( 0.000000000000000000, 1.000000000000000000, 0.000000000000000000 ) ) ;
#1099 = ORIENTED_EDGE ( 'NONE', *, *, #10096, .F. ) ;
#1100 = EDGE_CURVE ( 'NONE', #3973, #7049, #9351, .T. ) ;
#1101 = COLOUR_RGB ( '',1.000000000000000000, 0.9490196078431372140, 0.9098039215686274384 ) ;
#1102 = CARTESIAN_POINT ( 'NONE',  ( -61.73205080756886076, 10.44866454968463110, 2.500000000000003109 ) ) ;
#1103 = VECTOR ( 'NONE', #4447, 1000.000000000000000 ) ;
#1104 = VERTEX_POINT ( 'NONE', #7534 ) ;
#1105 = FACE_BOUND ( 'NONE', #1192, .T. ) ;
#1106 = ADVANCED_FACE ( 'NONE', ( #4968 ), #3304, .T. ) ;
#1107 = ADVANCED_FACE ( 'NONE', ( #10181 ), #10074, .F. ) ;
#1108 = CARTESIAN_POINT ( 'NONE',  ( -61.49999999999998579, 8.458333333333333925, 2.366025403784441927 ) ) ;
#1109 = DIRECTION ( 'NONE',  ( -0.000000000000000000, -1.000000000000000000, -0.000000000000000000 ) ) ;
#1110 = CARTESIAN_POINT ( 'NONE',  ( -139.9999999999999716, -43.00000000000000000, 3.000000000000000000 ) ) ;
#1111 = CARTESIAN_POINT ( 'NONE',  ( -46.99999999999998579, -18.00000000000001066, 0.000000000000000000 ) ) ;
#1112 = AXIS2_PLACEMENT_3D ( 'NONE', #9864, #10749, #426 ) ;
#1113 = CARTESIAN_POINT ( 'NONE',  ( -61.99999999999999289, 13.45312499965860376, 0.5015494609379544944 ) ) ;
#1114 = AXIS2_PLACEMENT_3D ( 'NONE', #2207, #7091, #483 ) ;
#1115 = CARTESIAN_POINT ( 'NONE',  ( -62.86468353124998742, 8.973958332991934128, 1.999225269531025972 ) ) ;
#1116 = CARTESIAN_POINT ( 'NONE',  ( -61.99999999999998579, 9.687500000000000000, 2.500000000000002665 ) ) ;
#1117 = CARTESIAN_POINT ( 'NONE',  ( -61.56765823437498142, 10.18229166632526805, 0.7511620957034663704 ) ) ;
#1118 = PLANE ( 'NONE',  #10139 ) ;
#1119 = VERTEX_POINT ( 'NONE', #3252 ) ;
#1120 = DIRECTION ( 'NONE',  ( -1.000000000000000000, 0.000000000000000000, 0.000000000000000000 ) ) ;
#1121 = CARTESIAN_POINT ( 'NONE',  ( -62.99999999999998579, 11.39583333333333393, 2.077350269189627952 ) ) ;
#1122 = CIRCLE ( 'NONE', #2538, 6.000000000000005329 ) ;
#1123 = CARTESIAN_POINT ( 'NONE',  ( -61.99999999999998579, 16.00000000000000000, 0.5000000000000041078 ) ) ;
#1124 = CARTESIAN_POINT ( 'NONE',  ( -61.56765823437498852, 12.53645833299193413, 2.248837904296538515 ) ) ;
#1125 = CARTESIAN_POINT ( 'NONE',  ( -62.43234176562499016, 8.494791666325268054, 2.248837904296538071 ) ) ;
#1126 = FACE_OUTER_BOUND ( 'NONE', #4388, .T. ) ;
#1127 = ORIENTED_EDGE ( 'NONE', *, *, #1789, .T. ) ;
#1128 = DIRECTION ( 'NONE',  ( 0.8571673013836855759, 1.049727191973305270E-16, -0.5150380737757257466 ) ) ;
#1129 = CARTESIAN_POINT ( 'NONE',  ( -61.99999999999999289, 9.953124999658601979, 0.5015494609379544944 ) ) ;
#1130 = DIRECTION ( 'NONE',  ( 0.000000000000000000, 0.000000000000000000, 1.000000000000000000 ) ) ;
#1131 = CARTESIAN_POINT ( 'NONE',  ( -62.86468353124998032, 15.18229166632526805, 1.000774730468978246 ) ) ;
#1132 = CARTESIAN_POINT ( 'NONE',  ( -61.99999999999998579, 14.15624999931720218, 2.654700538379254571 ) ) ;
#1133 = ORIENTED_EDGE ( 'NONE', *, *, #1752, .T. ) ;
#1134 = EDGE_CURVE ( 'NONE', #7831, #4618, #1812, .T. ) ;
#1135 = CARTESIAN_POINT ( 'NONE',  ( -105.0000000000000000, -2.500000000000000000, 4.000000000000000000 ) ) ;
#1136 = VERTEX_POINT ( 'NONE', #5803 ) ;
#1137 = ADVANCED_FACE ( 'NONE', ( #1695 ), #5069, .T. ) ;
#1138 = CARTESIAN_POINT ( 'NONE',  ( -61.99999999999999289, 12.39062499965860376, 0.5015494609379544944 ) ) ;
#1139 = CARTESIAN_POINT ( 'NONE',  ( -62.43234176562499016, 8.244791666325268054, 2.248837904296538071 ) ) ;
#1140 = DIRECTION ( 'NONE',  ( -0.000000000000000000, -1.000000000000000000, -0.000000000000000000 ) ) ;
#1141 = ORIENTED_EDGE ( 'NONE', *, *, #1332, .F. ) ;
#1142 = CARTESIAN_POINT ( 'NONE',  ( -60.99999999999998579, 12.52083333333333215, 0.9226497308103762673 ) ) ;
#1143 = CARTESIAN_POINT ( 'NONE',  ( -62.99999999999998579, 10.14583333333333570, 2.077350269189627952 ) ) ;
#1144 = CARTESIAN_POINT ( 'NONE',  ( -61.56765823437498142, 14.68229166632526805, 0.7511620957034663704 ) ) ;
#1145 = PRESENTATION_STYLE_ASSIGNMENT (( #3639 ) ) ;
#1146 = LINE ( 'NONE', #4527, #1576 ) ;
#1147 = CARTESIAN_POINT ( 'NONE',  ( -61.99999999999998579, 10.53124999931720396, 0.3452994616207497591 ) ) ;
#1148 = VERTEX_POINT ( 'NONE', #501 ) ;
#1149 = CARTESIAN_POINT ( 'NONE',  ( 1.299999999999999156, 0.000000000000000000, 0.000000000000000000 ) ) ;
#1150 = DIRECTION ( 'NONE',  ( 0.000000000000000000, -1.000000000000000000, 0.000000000000000000 ) ) ;
#1151 = CARTESIAN_POINT ( 'NONE',  ( -62.86468353124998032, 11.68229166632526805, 1.000774730468978246 ) ) ;
#1152 = SURFACE_STYLE_USAGE ( .BOTH. , #7105 ) ;
#1153 = ORIENTED_EDGE ( 'NONE', *, *, #10665, .F. ) ;
#1154 = EDGE_CURVE ( 'NONE', #5040, #5356, #5860, .T. ) ;
#1155 = CARTESIAN_POINT ( 'NONE',  ( -62.86468353124999453, 10.01562499965860198, 1.500000000000002220 ) ) ;
#1156 = CARTESIAN_POINT ( 'NONE',  ( -61.99999999999998579, 14.31250000000000000, 0.5000000000000013323 ) ) ;
#1157 = CARTESIAN_POINT ( 'NONE',  ( -61.56765823437498142, 14.93229166632526805, 0.7511620957034663704 ) ) ;
#1158 = CARTESIAN_POINT ( 'NONE',  ( -60.99999999999998579, 8.989583332650536107, 0.9226497308103762673 ) ) ;
#1159 = VERTEX_POINT ( 'NONE', #754 ) ;
#1160 = DIRECTION ( 'NONE',  ( -0.000000000000000000, -1.000000000000000000, -0.000000000000000000 ) ) ;
#1161 =( BOUNDED_CURVE ( )  B_SPLINE_CURVE ( 2, ( #5127, #7756, #2642, #10771, #5968, #910, #4240, #3161, #7702 ),
 .UNSPECIFIED., .F., .T. ) 
 B_SPLINE_CURVE_WITH_KNOTS ( ( 3, 2, 2, 2, 3 ),
 ( 0.6015625000000000000, 0.6041666666666666297, 0.6093750000000000000, 0.6145833333333333703, 0.6171875000000000000 ),
 .UNSPECIFIED. ) 
 CURVE ( )  GEOMETRIC_REPRESENTATION_ITEM ( )  RATIONAL_B_SPLINE_CURVE ( ( 0.9330127018922194093, 0.9330127018922194093, 1.000000000000000000, 0.8660254037844387076, 1.000000000000000000, 0.8660254037844387076, 1.000000000000000000, 0.9330127018922194093, 0.9330127018922194093 ) ) 
 REPRESENTATION_ITEM ( '' )  );
#1162 = ORIENTED_EDGE ( 'NONE', *, *, #6843, .F. ) ;
#1163 = PLANE ( 'NONE',  #7675 ) ;
#1164 = CARTESIAN_POINT ( 'NONE',  ( -62.49999999999998579, 9.083333333333333925, 0.6339745962155627357 ) ) ;
#1165 = DIRECTION ( 'NONE',  ( -1.000000000000000000, 0.000000000000000000, -0.000000000000000000 ) ) ;
#1166 = EDGE_CURVE ( 'NONE', #6004, #424, #5332, .T. ) ;
#1167 = FACE_OUTER_BOUND ( 'NONE', #6254, .T. ) ;
#1168 = CARTESIAN_POINT ( 'NONE',  ( -61.99999999999999289, 14.57812499965860198, 2.498450539062049724 ) ) ;
#1169 = CARTESIAN_POINT ( 'NONE',  ( -61.56765823437498852, 10.03645833299193413, 2.248837904296538515 ) ) ;
#1170 = UNCERTAINTY_MEASURE_WITH_UNIT (LENGTH_MEASURE( 1.000000000000000082E-05 ), #8148, 'distance_accuracy_value', 'NONE');
#1171 = CARTESIAN_POINT ( 'NONE',  ( -60.99999999999998579, 11.96874999931720218, 1.500000000000002220 ) ) ;
#1172 = CARTESIAN_POINT ( 'NONE',  ( -61.99999999999998579, 14.99999999999998579, 2.500000000000003109 ) ) ;
#1173 = CARTESIAN_POINT ( 'NONE',  ( -62.43234176562498305, 10.97395833299193590, 0.7511620957034662593 ) ) ;
#1174 = CARTESIAN_POINT ( 'NONE',  ( -62.26794919243111082, 13.57366454968463110, 0.5000000000000013323 ) ) ;
#1175 = VERTEX_POINT ( 'NONE', #1533 ) ;
#1176 = CARTESIAN_POINT ( 'NONE',  ( -61.73205080756886076, 14.02008544963257286, 0.5000000000000014433 ) ) ;
#1177 = EDGE_CURVE ( 'NONE', #4305, #2837, #8754, .T. ) ;
#1178 = CARTESIAN_POINT ( 'NONE',  ( -61.99999999999998579, 13.15624999931720218, 2.500000000000002665 ) ) ;
#1179 = VERTEX_POINT ( 'NONE', #1972 ) ;
#1180 = CARTESIAN_POINT ( 'NONE',  ( -61.99999999999998579, 16.00000000000000000, 0.5000000000000041078 ) ) ;
#1181 = CARTESIAN_POINT ( 'NONE',  ( -61.99999999999998579, 13.14062499965860198, 0.5015494609379544944 ) ) ;
#1182 = CARTESIAN_POINT ( 'NONE',  ( -61.13531646874997705, 8.557291666325268054, 1.999225269531026417 ) ) ;
#1183 = LINE ( 'NONE', #2138, #284 ) ;
#1184 = ORIENTED_EDGE ( 'NONE', *, *, #3450, .F. ) ;
#1185 = CARTESIAN_POINT ( 'NONE',  ( -61.99999999999998579, 15.93750000000000000, 2.654700538379254571 ) ) ;
#1186 = CARTESIAN_POINT ( 'NONE',  ( -62.86468353124999453, 9.786458332991934128, 1.999225269531025750 ) ) ;
#1187 = CARTESIAN_POINT ( 'NONE',  ( -61.99999999999998579, 15.39062499965860198, 0.5015494609379544944 ) ) ;
#1188 = CARTESIAN_POINT ( 'NONE',  ( -62.49999999999998579, 14.38541666598387003, 2.366025403784441483 ) ) ;
#1189 = CARTESIAN_POINT ( 'NONE',  ( -61.99999999999998579, 14.65624999931719863, 2.500000000000002665 ) ) ;
#1190 = VERTEX_POINT ( 'NONE', #6192 ) ;
#1191 = FACE_OUTER_BOUND ( 'NONE', #4245, .T. ) ;
#1192 = EDGE_LOOP ( 'NONE', ( #4332, #9103, #1729, #5757 ) ) ;
#1193 = CARTESIAN_POINT ( 'NONE',  ( -61.13531646874997705, 12.30729166632526628, 1.999225269531026417 ) ) ;
#1194 = CARTESIAN_POINT ( 'NONE',  ( -62.86468353124998032, 8.182291666325269830, 1.000774730468978246 ) ) ;
#1195 = SHAPE_REPRESENTATION ( 'dial indicator', ( #2307 ), #6386 ) ;
#1196 = CARTESIAN_POINT ( 'NONE',  ( -61.99999999999998579, 15.15624999931720218, 2.500000000000002665 ) ) ;
#1197 = ORIENTED_EDGE ( 'NONE', *, *, #1892, .T. ) ;
#1198 = CARTESIAN_POINT ( 'NONE',  ( -62.99999999999998579, 12.60416666666666607, 0.9226497308103756012 ) ) ;
#1199 = CARTESIAN_POINT ( 'NONE',  ( -61.99999999999998579, 10.06250000000000000, 0.5000000000000013323 ) ) ;
#1200 = CARTESIAN_POINT ( 'NONE',  ( -61.13531646874998415, 13.66145833299193590, 1.000774730468978468 ) ) ;
#1201 =( NAMED_UNIT ( * ) SI_UNIT ( $, .STERADIAN. ) SOLID_ANGLE_UNIT ( ) );
#1202 = CARTESIAN_POINT ( 'NONE',  ( -61.99999999999998579, 16.00000000000000000, 2.500000000000000444 ) ) ;
#1203 = CARTESIAN_POINT ( 'NONE',  ( -60.99999999999998579, 10.21874999931720218, 1.500000000000002220 ) ) ;
#1204 = EDGE_CURVE ( 'NONE', #6502, #5311, #805, .T. ) ;
#1205 = ORIENTED_EDGE ( 'NONE', *, *, #7217, .F. ) ;
#1206 =( GEOMETRIC_REPRESENTATION_CONTEXT ( 3 ) GLOBAL_UNCERTAINTY_ASSIGNED_CONTEXT ( ( #10045 ) ) GLOBAL_UNIT_ASSIGNED_CONTEXT ( ( #6328, #8215, #10032 ) ) REPRESENTATION_CONTEXT ( 'NONE', 'WORKASPACE' ) );
#1207 = DIRECTION ( 'NONE',  ( -0.000000000000000000, -1.000000000000000000, -0.000000000000000000 ) ) ;
#1208 = DIRECTION ( 'NONE',  ( -0.000000000000000000, 0.000000000000000000, 1.000000000000000000 ) ) ;
#1209 = CARTESIAN_POINT ( 'NONE',  ( -61.13531646874998415, 12.80729166632526805, 1.999225269531026417 ) ) ;
#1210 = DIRECTION ( 'NONE',  ( -0.000000000000000000, -0.000000000000000000, -1.000000000000000000 ) ) ;
#1211 = VERTEX_POINT ( 'NONE', #9579 ) ;
#1212 = CARTESIAN_POINT ( 'NONE',  ( -61.99999999999998579, 10.45312499965860198, 0.5015494609379544944 ) ) ;
#1213 = CARTESIAN_POINT ( 'NONE',  ( -62.49999999999998579, 15.55208333265053611, 0.6339745962155627357 ) ) ;
#1214 = VECTOR ( 'NONE', #9599, 1000.000000000000000 ) ;
#1215 = CARTESIAN_POINT ( 'NONE',  ( -61.13531646874998415, 13.89062499965860198, 1.500000000000002220 ) ) ;
#1216 = CARTESIAN_POINT ( 'NONE',  ( -61.99999999999998579, 16.00000000000000000, 0.5000000000000041078 ) ) ;
#1217 = EDGE_LOOP ( 'NONE', ( #6853, #818, #9578, #559 ) ) ;
#1218 = DIRECTION ( 'NONE',  ( -0.000000000000000000, -0.000000000000000000, -1.000000000000000000 ) ) ;
#1219 = ADVANCED_FACE ( 'NONE', ( #8526 ), #8695, .F. ) ;
#1220 = AXIS2_PLACEMENT_3D ( 'NONE', #10264, #8446, #2672 ) ;
#1221 = VECTOR ( 'NONE', #1539, 1000.000000000000000 ) ;
#1222 = ORIENTED_EDGE ( 'NONE', *, *, #4211, .F. ) ;
#1223 = PLANE ( 'NONE',  #592 ) ;
#1224 = CARTESIAN_POINT ( 'NONE',  ( -60.99999999999998579, 8.770833333333333925, 0.9226497308103762673 ) ) ;
#1225 = CARTESIAN_POINT ( 'NONE',  ( -62.99999999999998579, 9.593749999317202182, 1.500000000000001998 ) ) ;
#1226 = FACE_OUTER_BOUND ( 'NONE', #5077, .T. ) ;
#1227 = CARTESIAN_POINT ( 'NONE',  ( -149.9999999999999716, -8.000000000000000000, 3.000000000000000000 ) ) ;
#1228 = CARTESIAN_POINT ( 'NONE',  ( -61.13531646874997705, 14.86979166632526805, 1.999225269531026417 ) ) ;
#1229 = CARTESIAN_POINT ( 'NONE',  ( -61.13531646874998415, 9.578124999658600203, 1.500000000000002220 ) ) ;
#1230 = CARTESIAN_POINT ( 'NONE',  ( -149.9999999999999716, 8.000000000000000000, 3.000000000000000000 ) ) ;
#1231 = CARTESIAN_POINT ( 'NONE',  ( -62.43234176562499016, 11.05729166632526805, 2.248837904296538071 ) ) ;
#1232 = STYLED_ITEM ( 'NONE', ( #2645 ), #7886 ) ;
#1233 = CARTESIAN_POINT ( 'NONE',  ( -62.99999999999998579, 13.62500000000000000, 1.500000000000001998 ) ) ;
#1234 = EDGE_LOOP ( 'NONE', ( #6576, #8997, #7608, #685, #8217, #3108 ) ) ;
#1235 =( BOUNDED_CURVE ( )  B_SPLINE_CURVE ( 2, ( #2228, #3944, #10497, #7288, #1225, #10608, #2896, #394, #2117 ),
 .UNSPECIFIED., .F., .T. ) 
 B_SPLINE_CURVE_WITH_KNOTS ( ( 3, 2, 2, 2, 3 ),
 ( 0.1640624999999999722, 0.1666666666666666574, 0.1718750000000000000, 0.1770833333333333426, 0.1796875000000000555 ),
 .UNSPECIFIED. ) 
 CURVE ( )  GEOMETRIC_REPRESENTATION_ITEM ( )  RATIONAL_B_SPLINE_CURVE ( ( 0.9330127018922194093, 0.9330127018922186322, 1.000000000000000000, 0.8660254037844387076, 1.000000000000000000, 0.8660254037844387076, 1.000000000000000000, 0.9330127018922178550, 0.9330127018922192983 ) ) 
 REPRESENTATION_ITEM ( '' )  );
#1236 = DIRECTION ( 'NONE',  ( -0.000000000000000000, -0.000000000000000000, 1.000000000000000000 ) ) ;
#1237 = CARTESIAN_POINT ( 'NONE',  ( -62.49999999999998579, 9.083333333333333925, 0.6339745962155627357 ) ) ;
#1238 = AXIS2_PLACEMENT_3D ( 'NONE', #948, #9504, #8510 ) ;
#1239 = VERTEX_POINT ( 'NONE', #129 ) ;
#1240 = CARTESIAN_POINT ( 'NONE',  ( -61.99999999999998579, 10.15624999931720041, 2.500000000000002665 ) ) ;
#1241 = CARTESIAN_POINT ( 'NONE',  ( -61.99999999999998579, 12.89062499965860376, 0.5015494609379544944 ) ) ;
#1242 = CARTESIAN_POINT ( 'NONE',  ( -61.13531646874997705, 10.05729166632526983, 1.999225269531026417 ) ) ;
#1243 = PRESENTATION_LAYER_ASSIGNMENT (  '', '', ( #10823 ) ) ;
#1244 = DIRECTION ( 'NONE',  ( -1.000000000000000000, 0.000000000000000000, 0.000000000000000000 ) ) ;
#1245 = VERTEX_POINT ( 'NONE', #1074 ) ;
#1246 = CARTESIAN_POINT ( 'NONE',  ( -61.99999999999998579, 14.06250000000000000, 0.5000000000000013323 ) ) ;
#1247 = CARTESIAN_POINT ( 'NONE',  ( -62.43234176562499016, 12.05729166632526628, 2.248837904296538071 ) ) ;
#1248 = APPLICATION_PROTOCOL_DEFINITION ( 'draft international standard', 'automotive_design', 1998, #1873 ) ;
#1249 = CARTESIAN_POINT ( 'NONE',  ( -61.99999999999998579, 15.76562499965860020, 2.498450539062049724 ) ) ;
#1250 = AXIS2_PLACEMENT_3D ( 'NONE', #6279, #1542, #9834 ) ;
#1251 = CARTESIAN_POINT ( 'NONE',  ( -61.49999999999998579, 15.01041666598386826, 0.6339745962155628467 ) ) ;
#1252 = DIRECTION ( 'NONE',  ( -1.000000000000000000, 0.000000000000000000, -0.000000000000000000 ) ) ;
#1253 = VERTEX_POINT ( 'NONE', #10230 ) ;
#1254 = CARTESIAN_POINT ( 'NONE',  ( -61.99999999999998579, 15.28124999931720218, 0.5000000000000013323 ) ) ;
#1255 = ORIENTED_EDGE ( 'NONE', *, *, #3655, .T. ) ;
#1256 = MECHANICAL_DESIGN_GEOMETRIC_PRESENTATION_REPRESENTATION (  '', ( #365 ), #3726 ) ;
#1257 = CARTESIAN_POINT ( 'NONE',  ( -61.13531646874997705, 12.84895833299193413, 1.000774730468978468 ) ) ;
#1258 = CARTESIAN_POINT ( 'NONE',  ( -62.43234176562498305, 8.661458332991934128, 0.7511620957034662593 ) ) ;
#1259 = DIRECTION ( 'NONE',  ( -0.000000000000000000, -1.000000000000000000, -0.000000000000000000 ) ) ;
#1260 = VERTEX_POINT ( 'NONE', #3461 ) ;
#1261 = CARTESIAN_POINT ( 'NONE',  ( -62.99999999999998579, 11.89583333333333215, 2.077350269189627952 ) ) ;
#1262 = ADVANCED_FACE ( 'NONE', ( #3631 ), #961, .F. ) ;
#1263 = CARTESIAN_POINT ( 'NONE',  ( -61.49999999999998579, 15.92708333265053433, 2.366025403784441927 ) ) ;
#1264 = CARTESIAN_POINT ( 'NONE',  ( -62.43234176562499016, 14.05729166632526805, 2.248837904296538071 ) ) ;
#1265 = SURFACE_SIDE_STYLE ('',( #8878 ) ) ;
#1266 = CARTESIAN_POINT ( 'NONE',  ( -62.99999999999998579, 14.32291666598387003, 0.9226497308103756012 ) ) ;
#1267 = CARTESIAN_POINT ( 'NONE',  ( -60.99999999999998579, 9.947916665983868256, 2.077350269189628840 ) ) ;
#1268 = VERTEX_POINT ( 'NONE', #904 ) ;
#1269 = CARTESIAN_POINT ( 'NONE',  ( -61.99999999999998579, 15.40624999931720218, 2.500000000000002665 ) ) ;
#1270 = CARTESIAN_POINT ( 'NONE',  ( -61.56765823437498852, 12.28645833299193413, 2.248837904296538515 ) ) ;
#1271 = CARTESIAN_POINT ( 'NONE',  ( -9.262305278225771052E-15, -0.2499999999999999445, 1.454152683131084256 ) ) ;
#1272 = ADVANCED_FACE ( 'NONE', ( #8756 ), #189, .T. ) ;
#1273 = EDGE_LOOP ( 'NONE', ( #7281, #1401 ) ) ;
#1274 = CARTESIAN_POINT ( 'NONE',  ( -61.13531646874998415, 10.16145833299193413, 1.000774730468978468 ) ) ;
#1275 = FACE_OUTER_BOUND ( 'NONE', #6489, .T. ) ;
#1276 = CARTESIAN_POINT ( 'NONE',  ( -61.13531646874998415, 15.89062499965860198, 1.500000000000002220 ) ) ;
#1277 = CARTESIAN_POINT ( 'NONE',  ( -61.99999999999998579, 26.00000000000000355, 4.000000000000004441 ) ) ;
#1278 = EDGE_LOOP ( 'NONE', ( #2312, #1859, #4529, #3092 ) ) ;
#1279 = FACE_OUTER_BOUND ( 'NONE', #6316, .T. ) ;
#1280 = EDGE_CURVE ( 'NONE', #10017, #2164, #4461, .T. ) ;
#1281 = EDGE_CURVE ( 'NONE', #10876, #5522, #9466, .T. ) ;
#1282 = ORIENTED_EDGE ( 'NONE', *, *, #6378, .T. ) ;
#1283 = CARTESIAN_POINT ( 'NONE',  ( -62.49999999999998579, 15.13541666598387003, 2.366025403784441483 ) ) ;
#1284 = CARTESIAN_POINT ( 'NONE',  ( -62.49999999999998579, 10.08333333333333215, 0.6339745962155627357 ) ) ;
#1285 = LINE ( 'NONE', #8070, #10882 ) ;
#1286 = DIRECTION ( 'NONE',  ( 1.000000000000000000, 0.000000000000000000, 0.000000000000000000 ) ) ;
#1287 = CARTESIAN_POINT ( 'NONE',  ( -60.99999999999998579, 10.71874999931720396, 1.500000000000002220 ) ) ;
#1288 = EDGE_CURVE ( 'NONE', #5990, #4251, #8584, .T. ) ;
#1289 = CARTESIAN_POINT ( 'NONE',  ( -61.13531646874998415, 10.05729166632526983, 1.999225269531026417 ) ) ;
#1290 = CARTESIAN_POINT ( 'NONE',  ( -61.99999999999998579, 16.00000000000000000, 2.500000000000000444 ) ) ;
#1291 = CARTESIAN_POINT ( 'NONE',  ( 0.5000000000000000000, -0.2499999999999997780, -2.000000000000000000 ) ) ;
#1292 = AXIS2_PLACEMENT_3D ( 'NONE', #7583, #3406, #9982 ) ;
#1293 = CARTESIAN_POINT ( 'NONE',  ( -62.86468353124998032, 10.24479166632526983, 1.000774730468978246 ) ) ;
#1294 = DIRECTION ( 'NONE',  ( 0.000000000000000000, 0.000000000000000000, 1.000000000000000000 ) ) ;
#1295 = PRODUCT_RELATED_PRODUCT_CATEGORY ( 'part', '', ( #48 ) ) ;
#1296 = VERTEX_POINT ( 'NONE', #1135 ) ;
#1297 = CARTESIAN_POINT ( 'NONE',  ( -77.99999999999998579, -11.50000000000000711, 4.999999999999999112 ) ) ;
#1298 = PRODUCT_DEFINITION_CONTEXT ( 'detailed design', #6771, 'design' ) ;
#1299 = CARTESIAN_POINT ( 'NONE',  ( -61.99999999999998579, 16.00000000000000000, 2.500000000000000444 ) ) ;
#1300 = ORIENTED_EDGE ( 'NONE', *, *, #4359, .T. ) ;
#1301 = CARTESIAN_POINT ( 'NONE',  ( -60.99999999999998579, 10.21874999931720218, 1.500000000000002220 ) ) ;
#1302 = CARTESIAN_POINT ( 'NONE',  ( -62.86468353124999453, 12.95312499965860198, 1.500000000000002220 ) ) ;
#1303 = CARTESIAN_POINT ( 'NONE',  ( -61.13531646874997705, 10.09895833299193413, 1.000774730468978468 ) ) ;
#1304 = PLANE ( 'NONE',  #10493 ) ;
#1305 = ORIENTED_EDGE ( 'NONE', *, *, #1734, .F. ) ;
#1306 = CARTESIAN_POINT ( 'NONE',  ( -76.99999999999998579, -11.50000000000000711, 8.000000000000000000 ) ) ;
#1307 = CARTESIAN_POINT ( 'NONE',  ( -62.43234176562499016, 10.80729166632526805, 2.248837904296538071 ) ) ;
#1308 = ADVANCED_FACE ( 'NONE', ( #7920 ), #301, .T. ) ;
#1309 = SHAPE_DEFINITION_REPRESENTATION ( #5090, #1195 ) ;
#1310 = CARTESIAN_POINT ( 'NONE',  ( -61.56765823437498852, 15.03645833299193590, 2.248837904296538515 ) ) ;
#1311 = CARTESIAN_POINT ( 'NONE',  ( -61.99999999999998579, 14.40624999931720218, 2.654700538379254571 ) ) ;
#1312 = DIRECTION ( 'NONE',  ( 0.000000000000000000, 0.000000000000000000, 1.000000000000000000 ) ) ;
#1313 = ORIENTED_EDGE ( 'NONE', *, *, #1429, .T. ) ;
#1314 = AXIS2_PLACEMENT_3D ( 'NONE', #8865, #8146, #1252 ) ;
#1315 = CARTESIAN_POINT ( 'NONE',  ( -61.99999999999998579, 13.53124999931720041, 0.5000000000000013323 ) ) ;
#1316 = EDGE_LOOP ( 'NONE', ( #2338, #10742, #637, #5601 ) ) ;
#1317 = EDGE_CURVE ( 'NONE', #4292, #7283, #10867, .T. ) ;
#1318 = CARTESIAN_POINT ( 'NONE',  ( -61.56765823437498142, 13.11979166632526805, 0.7511620957034663704 ) ) ;
#1319 = CARTESIAN_POINT ( 'NONE',  ( -61.99999999999998579, 8.640624999658601979, 0.5015494609379544944 ) ) ;
#1320 = FACE_OUTER_BOUND ( 'NONE', #2407, .T. ) ;
#1321 = MANIFOLD_SOLID_BREP ( 'Cavity1', #4988 ) ;
#1322 = ORIENTED_EDGE ( 'NONE', *, *, #943, .F. ) ;
#1323 = CARTESIAN_POINT ( 'NONE',  ( -60.99999999999998579, 12.27083333333333393, 0.9226497308103762673 ) ) ;
#1324 = VECTOR ( 'NONE', #9947, 1000.000000000000000 ) ;
#1325 = CARTESIAN_POINT ( 'NONE',  ( -62.26794919243111082, 13.39508544963257286, 2.500000000000003109 ) ) ;
#1326 = EDGE_CURVE ( 'NONE', #869, #5526, #7085, .T. ) ;
#1327 = SURFACE_STYLE_USAGE ( .BOTH. , #1265 ) ;
#1328 = CARTESIAN_POINT ( 'NONE',  ( 143.9000000000000341, 5.500000000000000000, 6.000000000000000000 ) ) ;
#1329 = CARTESIAN_POINT ( 'NONE',  ( -61.99999999999998579, 10.03124999931720396, 0.3452994616207497591 ) ) ;
#1330 = VERTEX_POINT ( 'NONE', #1315 ) ;
#1331 = DIRECTION ( 'NONE',  ( 0.000000000000000000, 0.000000000000000000, 1.000000000000000000 ) ) ;
#1332 = EDGE_CURVE ( 'NONE', #1179, #3194, #927, .T. ) ;
#1333 = CARTESIAN_POINT ( 'NONE',  ( -62.86468353124999453, 12.70312499965860198, 1.500000000000002220 ) ) ;
#1334 = FACE_OUTER_BOUND ( 'NONE', #6161, .T. ) ;
#1335 = ORIENTED_EDGE ( 'NONE', *, *, #5192, .T. ) ;
#1336 = CARTESIAN_POINT ( 'NONE',  ( -61.56765823437498852, 11.34895833299193590, 2.248837904296538515 ) ) ;
#1337 = CARTESIAN_POINT ( 'NONE',  ( -61.99999999999998579, 13.03124999931720218, 0.5000000000000013323 ) ) ;
#1338 = CARTESIAN_POINT ( 'NONE',  ( -61.56765823437498142, 15.68229166632526628, 0.7511620957034663704 ) ) ;
#1339 = CARTESIAN_POINT ( 'NONE',  ( -61.99999999999998579, 9.031249999317202182, 0.5000000000000013323 ) ) ;
#1340 = EDGE_LOOP ( 'NONE', ( #238, #5363, #5092, #7261, #4256, #4767, #7735, #1853 ) ) ;
#1341 = DIRECTION ( 'NONE',  ( -1.734723475976807094E-15, 1.000000000000000000, 0.000000000000000000 ) ) ;
#1342 = ORIENTED_EDGE ( 'NONE', *, *, #7597, .T. ) ;
#1343 = DIRECTION ( 'NONE',  ( -0.000000000000000000, -1.000000000000000000, -0.000000000000000000 ) ) ;
#1344 = CARTESIAN_POINT ( 'NONE',  ( -62.99999999999998579, 9.645833333333332149, 2.077350269189627952 ) ) ;
#1345 = DIRECTION ( 'NONE',  ( -0.000000000000000000, 0.000000000000000000, 1.000000000000000000 ) ) ;
#1346 = CARTESIAN_POINT ( 'NONE',  ( -61.99999999999998579, 10.28124999931720218, 0.5000000000000013323 ) ) ;
#1347 = CARTESIAN_POINT ( 'NONE',  ( -60.99999999999998579, 8.270833333333333925, 0.9226497308103762673 ) ) ;
#1348 = EDGE_CURVE ( 'NONE', #4452, #8833, #3865, .T. ) ;
#1349 = CARTESIAN_POINT ( 'NONE',  ( -61.13531646874998415, 10.55729166632526805, 1.999225269531026417 ) ) ;
#1350 = LINE ( 'NONE', #3214, #9205 ) ;
#1351 = CARTESIAN_POINT ( 'NONE',  ( -62.43234176562499016, 12.30729166632526805, 2.248837904296538071 ) ) ;
#1352 = EDGE_CURVE ( 'NONE', #2202, #2668, #7554, .T. ) ;
#1353 = DIRECTION ( 'NONE',  ( 0.000000000000000000, 1.000000000000000000, 0.000000000000000000 ) ) ;
#1354 = ORIENTED_EDGE ( 'NONE', *, *, #2995, .F. ) ;
#1355 = DIRECTION ( 'NONE',  ( -0.000000000000000000, -0.000000000000000000, 1.000000000000000000 ) ) ;
#1356 = FACE_BOUND ( 'NONE', #8492, .T. ) ;
#1357 = ORIENTED_EDGE ( 'NONE', *, *, #8744, .F. ) ;
#1358 = CARTESIAN_POINT ( 'NONE',  ( -62.99999999999998579, 10.09374999931720218, 1.500000000000001998 ) ) ;
#1359 = CARTESIAN_POINT ( 'NONE',  ( -62.43234176562498305, 13.66145833299193413, 0.7511620957034662593 ) ) ;
#1360 = CARTESIAN_POINT ( 'NONE',  ( -62.86468353124999453, 10.47395833299193235, 1.999225269531025750 ) ) ;
#1361 = PRESENTATION_STYLE_ASSIGNMENT (( #5513 ) ) ;
#1362 = ORIENTED_EDGE ( 'NONE', *, *, #2808, .F. ) ;
#1363 = CARTESIAN_POINT ( 'NONE',  ( -61.99999999999998579, 11.43750000000000000, 2.500000000000002665 ) ) ;
#1364 = CARTESIAN_POINT ( 'NONE',  ( -62.86468353124998032, 10.74479166632526805, 1.000774730468978024 ) ) ;
#1365 = CARTESIAN_POINT ( 'NONE',  ( -62.99999999999998579, 15.14583333333333215, 2.077350269189627952 ) ) ;
#1366 = CARTESIAN_POINT ( 'NONE',  ( -62.49999999999998579, 16.05208333265053255, 0.6339745962155627357 ) ) ;
#1367 = CARTESIAN_POINT ( 'NONE',  ( -61.99999999999998579, 14.78124999931720218, 0.5000000000000013323 ) ) ;
#1368 = ORIENTED_EDGE ( 'NONE', *, *, #367, .T. ) ;
#1369 =( NAMED_UNIT ( * ) PLANE_ANGLE_UNIT ( ) SI_UNIT ( $, .RADIAN. ) );
#1370 = EDGE_LOOP ( 'NONE', ( #6623, #417, #8003, #8924 ) ) ;
#1371 = EDGE_CURVE ( 'NONE', #2202, #3478, #5006, .T. ) ;
#1372 = CARTESIAN_POINT ( 'NONE',  ( -62.86468353124998032, 12.93229166632526805, 1.000774730468978024 ) ) ;
#1373 = CARTESIAN_POINT ( 'NONE',  ( -61.99999999999998579, 10.26562499965860376, 2.498450539062049724 ) ) ;
#1374 = ORIENTED_EDGE ( 'NONE', *, *, #2836, .T. ) ;
#1375 = CARTESIAN_POINT ( 'NONE',  ( -61.49999999999998579, 13.04166666666666607, 0.6339745962155628467 ) ) ;
#1376 = CARTESIAN_POINT ( 'NONE',  ( 11.30000000000000426, 0.000000000000000000, 1.000000000000000000 ) ) ;
#1377 = CARTESIAN_POINT ( 'NONE',  ( -62.99999999999998579, 11.07291666598386826, 0.9226497308103756012 ) ) ;
#1378 = CARTESIAN_POINT ( 'NONE',  ( -61.99999999999998579, 13.43749999999999822, 2.500000000000002665 ) ) ;
#1379 = CARTESIAN_POINT ( 'NONE',  ( -62.43234176562499016, 12.99479166632526805, 2.248837904296538071 ) ) ;
#1380 = CARTESIAN_POINT ( 'NONE',  ( -119.9999999999999858, 15.67949192431120053, 0.000000000000000000 ) ) ;
#1381 = EDGE_LOOP ( 'NONE', ( #2924, #6869, #5450, #5185 ) ) ;
#1382 = CARTESIAN_POINT ( 'NONE',  ( -61.56765823437498142, 10.93229166632526805, 0.7511620957034663704 ) ) ;
#1383 = CARTESIAN_POINT ( 'NONE',  ( -77.99999999999998579, 11.49999999999999645, 4.999999999999999112 ) ) ;
#1384 = EDGE_CURVE ( 'NONE', #8873, #9906, #9440, .T. ) ;
#1385 = AXIS2_PLACEMENT_3D ( 'NONE', #7652, #1150, #7993 ) ;
#1386 = CARTESIAN_POINT ( 'NONE',  ( -61.99999999999998579, 15.57812499965860198, 2.498450539062049724 ) ) ;
#1387 = ORIENTED_EDGE ( 'NONE', *, *, #3636, .T. ) ;
#1388 = DIRECTION ( 'NONE',  ( -0.000000000000000000, 1.000000000000000000, -0.000000000000000000 ) ) ;
#1389 = VECTOR ( 'NONE', #1722, 1000.000000000000000 ) ;
#1390 = ORIENTED_EDGE ( 'NONE', *, *, #8995, .F. ) ;
#1391 = CARTESIAN_POINT ( 'NONE',  ( -43.00000000000000711, -14.00000000000000888, 5.000000000000000000 ) ) ;
#1392 = CARTESIAN_POINT ( 'NONE',  ( -62.99999999999998579, 9.395833333333333925, 2.077350269189627952 ) ) ;
#1393 = CARTESIAN_POINT ( 'NONE',  ( -61.49999999999998579, 11.29166666666666607, 0.6339745962155628467 ) ) ;
#1394 = DIRECTION ( 'NONE',  ( 0.000000000000000000, 0.000000000000000000, -1.000000000000000000 ) ) ;
#1395 = CARTESIAN_POINT ( 'NONE',  ( -62.49999999999998579, 14.80208333265053611, 0.6339745962155627357 ) ) ;
#1396 =( BOUNDED_CURVE ( )  B_SPLINE_CURVE ( 2, ( #7764, #145, #6149, #10482, #6326, #9655, #261, #3644, #1269 ),
 .UNSPECIFIED., .F., .T. ) 
 B_SPLINE_CURVE_WITH_KNOTS ( ( 3, 2, 2, 2, 3 ),
 ( 0.8828125000000000000, 0.8854166666666666297, 0.8906250000000000000, 0.8958333333333333703, 0.8984375000000000000 ),
 .UNSPECIFIED. ) 
 CURVE ( )  GEOMETRIC_REPRESENTATION_ITEM ( )  RATIONAL_B_SPLINE_CURVE ( ( 0.9330127018922194093, 0.9330127018922194093, 1.000000000000000000, 0.8660254037844387076, 1.000000000000000000, 0.8660254037844387076, 1.000000000000000000, 0.9330127018922194093, 0.9330127018922194093 ) ) 
 REPRESENTATION_ITEM ( '' )  );
#1397 = CARTESIAN_POINT ( 'NONE',  ( -62.99999999999998579, 8.364583332650536107, 2.077350269189627952 ) ) ;
#1398 = VECTOR ( 'NONE', #3895, 1000.000000000000000 ) ;
#1399 = CARTESIAN_POINT ( 'NONE',  ( -61.56765823437498142, 11.43229166632526805, 0.7511620957034663704 ) ) ;
#1400 = DIRECTION ( 'NONE',  ( 0.000000000000000000, 0.000000000000000000, 1.000000000000000000 ) ) ;
#1401 = ORIENTED_EDGE ( 'NONE', *, *, #1177, .T. ) ;
#1402 = CARTESIAN_POINT ( 'NONE',  ( -61.73205080756886076, 9.270085449632572860, 0.5000000000000014433 ) ) ;
#1403 = DIRECTION ( 'NONE',  ( 0.000000000000000000, 0.000000000000000000, -1.000000000000000000 ) ) ;
#1404 = AXIS2_PLACEMENT_3D ( 'NONE', #1447, #3009, #5714 ) ;
#1405 = VERTEX_POINT ( 'NONE', #2148 ) ;
#1406 = CARTESIAN_POINT ( 'NONE',  ( -61.73205080756886076, 14.16741454900183328, 2.500000000000003109 ) ) ;
#1407 = CARTESIAN_POINT ( 'NONE',  ( -61.13531646874998415, 14.30729166632526983, 1.999225269531026417 ) ) ;
#1408 = ADVANCED_FACE ( 'NONE', ( #3035, #5581 ), #9694, .F. ) ;
#1409 = CARTESIAN_POINT ( 'NONE',  ( -62.43234176562499016, 10.49479166632526983, 2.248837904296538071 ) ) ;
#1410 = CARTESIAN_POINT ( 'NONE',  ( -120.0000000000000000, -8.000000000000000000, -2.000000000000000000 ) ) ;
#1411 = ORIENTED_EDGE ( 'NONE', *, *, #9974, .F. ) ;
#1412 = DIRECTION ( 'NONE',  ( -1.000000000000000000, 0.000000000000000000, -0.000000000000000000 ) ) ;
#1413 = CARTESIAN_POINT ( 'NONE',  ( -62.86468353124999453, 11.03645833299193590, 1.999225269531025750 ) ) ;
#1414 = CIRCLE ( 'NONE', #10446, 1.934182851860891672 ) ;
#1415 = DIRECTION ( 'NONE',  ( -1.000000000000000000, -0.000000000000000000, -0.000000000000000000 ) ) ;
#1416 = CARTESIAN_POINT ( 'NONE',  ( -60.99999999999998579, 15.73958333265053611, 0.9226497308103762673 ) ) ;
#1417 = CARTESIAN_POINT ( 'NONE',  ( -109.9999999999999574, 14.99999999999998579, -2.000000000000000000 ) ) ;
#1418 = ORIENTED_EDGE ( 'NONE', *, *, #771, .F. ) ;
#1419 = PLANE ( 'NONE',  #8329 ) ;
#1420 = LINE ( 'NONE', #7253, #4126 ) ;
#1421 = AXIS2_PLACEMENT_3D ( 'NONE', #4124, #10850, #4069 ) ;
#1422 = CARTESIAN_POINT ( 'NONE',  ( -62.43234176562498305, 14.16145833299193413, 0.7511620957034662593 ) ) ;
#1423 = CARTESIAN_POINT ( 'NONE',  ( -61.56765823437498142, 10.11979166632526805, 0.7511620957034663704 ) ) ;
#1424 = CARTESIAN_POINT ( 'NONE',  ( -60.99999999999998579, 16.10937499965860198, 1.500000000000002220 ) ) ;
#1425 = ORIENTED_EDGE ( 'NONE', *, *, #9158, .F. ) ;
#1426 = CARTESIAN_POINT ( 'NONE',  ( -61.49999999999998579, 14.29166666666666785, 0.6339745962155628467 ) ) ;
#1427 = AXIS2_PLACEMENT_3D ( 'NONE', #2719, #9226, #8549 ) ;
#1428 = PRESENTATION_STYLE_ASSIGNMENT (( #435 ) ) ;
#1429 = EDGE_CURVE ( 'NONE', #7720, #9736, #1420, .T. ) ;
#1430 = CARTESIAN_POINT ( 'NONE',  ( -62.49999999999998579, 11.63541666598387003, 2.366025403784441483 ) ) ;
#1431 = MECHANICAL_DESIGN_GEOMETRIC_PRESENTATION_REPRESENTATION (  '', ( #4072 ), #10650 ) ;
#1432 = PRODUCT_RELATED_PRODUCT_CATEGORY ( 'part', '', ( #9011 ) ) ;
#1433 = CARTESIAN_POINT ( 'NONE',  ( -62.99999999999998579, 14.89583333333333925, 2.077350269189627952 ) ) ;
#1434 = AXIS2_PLACEMENT_3D ( 'NONE', #8540, #1762, #10194 ) ;
#1435 = CARTESIAN_POINT ( 'NONE',  ( -61.13531646874998415, 12.55729166632526805, 1.999225269531026417 ) ) ;
#1436 = EDGE_LOOP ( 'NONE', ( #3937, #4872, #1658, #9848 ) ) ;
#1437 = CARTESIAN_POINT ( 'NONE',  ( -62.43234176562498305, 11.97395833299193413, 0.7511620957034662593 ) ) ;
#1438 = FACE_OUTER_BOUND ( 'NONE', #10048, .T. ) ;
#1439 = CARTESIAN_POINT ( 'NONE',  ( -61.99999999999998579, 15.95312499965860198, 0.5015494609379544944 ) ) ;
#1440 = ORIENTED_EDGE ( 'NONE', *, *, #5121, .T. ) ;
#1441 = DIRECTION ( 'NONE',  ( -0.000000000000000000, -0.000000000000000000, -1.000000000000000000 ) ) ;
#1442 = ORIENTED_EDGE ( 'NONE', *, *, #8241, .F. ) ;
#1443 = CARTESIAN_POINT ( 'NONE',  ( -61.49999999999998579, 8.760416665983868256, 0.6339745962155628467 ) ) ;
#1444 = CARTESIAN_POINT ( 'NONE',  ( -61.49999999999998579, 9.291666666666666075, 0.6339745962155628467 ) ) ;
#1445 = DIRECTION ( 'NONE',  ( 1.000000000000000000, 0.000000000000000000, 0.000000000000000000 ) ) ;
#1446 = FACE_OUTER_BOUND ( 'NONE', #6334, .T. ) ;
#1447 = CARTESIAN_POINT ( 'NONE',  ( -77.99999999999998579, 11.49999999999999645, -2.000000000000001332 ) ) ;
#1448 = EDGE_CURVE ( 'NONE', #8888, #10687, #4798, .T. ) ;
#1449 = CARTESIAN_POINT ( 'NONE',  ( -62.99999999999998579, 8.343749999317202182, 1.500000000000001998 ) ) ;
#1450 = CARTESIAN_POINT ( 'NONE',  ( -62.86468353124998742, 12.03645833299193413, 1.999225269531025972 ) ) ;
#1451 = CARTESIAN_POINT ( 'NONE',  ( 0.5477065543514070267, 0.000000000000000000, 0.000000000000000000 ) ) ;
#1452 = VERTEX_POINT ( 'NONE', #9917 ) ;
#1453 = AXIS2_PLACEMENT_3D ( 'NONE', #1634, #2311, #10752 ) ;
#1454 = CARTESIAN_POINT ( 'NONE',  ( -77.99999999999998579, -11.50000000000000711, 8.600860617226443239 ) ) ;
#1455 = DIRECTION ( 'NONE',  ( -0.000000000000000000, -1.000000000000000000, -0.000000000000000000 ) ) ;
#1456 =( REPRESENTATION_RELATIONSHIP ('NONE','NONE', #560, #2047 ) REPRESENTATION_RELATIONSHIP_WITH_TRANSFORMATION ( #9911 )SHAPE_REPRESENTATION_RELATIONSHIP( ) );
#1457 = ADVANCED_FACE ( 'NONE', ( #4571 ), #6535, .T. ) ;
#1458 = FACE_OUTER_BOUND ( 'NONE', #2511, .T. ) ;
#1459 = CARTESIAN_POINT ( 'NONE',  ( -49.99999999999998579, -15.00000000000001243, 5.000000000000004441 ) ) ;
#1460 = CARTESIAN_POINT ( 'NONE',  ( -62.43234176562498305, 14.16145833299193413, 0.7511620957034662593 ) ) ;
#1461 = CARTESIAN_POINT ( 'NONE',  ( -61.99999999999999289, 10.26562499965860376, 2.498450539062049724 ) ) ;
#1462 =( NAMED_UNIT ( * ) PLANE_ANGLE_UNIT ( ) SI_UNIT ( $, .RADIAN. ) );
#1463 =( BOUNDED_CURVE ( )  B_SPLINE_CURVE ( 2, ( #9631, #3856, #2025, #4682, #418, #7137, #3741, #7856, #10519 ),
 .UNSPECIFIED., .F., .F. ) 
 B_SPLINE_CURVE_WITH_KNOTS ( ( 3, 2, 2, 2, 3 ),
 ( 0.02343749999999996531, 0.02604166666666666782, 0.03125000000000000000, 0.03645833333333333565, 0.03906250000000003469 ),
 .UNSPECIFIED. ) 
 CURVE ( )  GEOMETRIC_REPRESENTATION_ITEM ( )  RATIONAL_B_SPLINE_CURVE ( ( 0.9330127018922194093, 0.9330127018922185211, 1.000000000000000000, 0.8660254037844387076, 1.000000000000000000, 0.8660254037844387076, 1.000000000000000000, 0.9330127018922185211, 0.9330127018922194093 ) ) 
 REPRESENTATION_ITEM ( '' )  );
#1464 = CARTESIAN_POINT ( 'NONE',  ( -61.99999999999998579, 8.281249999317202182, 0.5000000000000013323 ) ) ;
#1465 = CIRCLE ( 'NONE', #4462, 6.000000000000005329 ) ;
#1466 = CARTESIAN_POINT ( 'NONE',  ( -61.56765823437498852, 11.34895833299193590, 2.248837904296538515 ) ) ;
#1467 = CARTESIAN_POINT ( 'NONE',  ( -61.13531646874998415, 8.098958332991934128, 1.000774730468978468 ) ) ;
#1468 = ITEM_DEFINED_TRANSFORMATION ( 'NONE', 'NONE', #5848,  #2307 ) ;
#1469 = LINE ( 'NONE', #9130, #2120 ) ;
#1470 = CARTESIAN_POINT ( 'NONE',  ( -61.13531646874998415, 8.390624999658601979, 1.500000000000002220 ) ) ;
#1471 = DIRECTION ( 'NONE',  ( 0.000000000000000000, 0.000000000000000000, -1.000000000000000000 ) ) ;
#1472 = ORIENTED_EDGE ( 'NONE', *, *, #9040, .T. ) ;
#1473 = CARTESIAN_POINT ( 'NONE',  ( 0.5999999999999999778, 0.000000000000000000, 0.000000000000000000 ) ) ;
#1474 = VECTOR ( 'NONE', #2291, 1000.000000000000000 ) ;
#1475 = CARTESIAN_POINT ( 'NONE',  ( -62.86468353124998032, 13.93229166632526805, 1.000774730468978024 ) ) ;
#1476 = CARTESIAN_POINT ( 'NONE',  ( -61.56765823437498142, 9.369791666325268054, 0.7511620957034663704 ) ) ;
#1477 = CARTESIAN_POINT ( 'NONE',  ( -61.99999999999998579, 10.43750000000000000, 2.500000000000002665 ) ) ;
#1478 = ORIENTED_EDGE ( 'NONE', *, *, #4677, .F. ) ;
#1479 = CARTESIAN_POINT ( 'NONE',  ( -62.49999999999998579, 14.33333333333333393, 0.6339745962155627357 ) ) ;
#1480 = PRODUCT_DEFINITION_SHAPE ( 'NONE', 'NONE',  #3253 ) ;
#1481 = DIRECTION ( 'NONE',  ( -3.965082230804130220E-16, 1.000000000000000000, 0.000000000000000000 ) ) ;
#1482 = AXIS2_PLACEMENT_3D ( 'NONE', #3684, #9465, #6135 ) ;
#1483 = ADVANCED_FACE ( 'NONE', ( #1191 ), #4634, .T. ) ;
#1484 = CARTESIAN_POINT ( 'NONE',  ( -61.99999999999998579, 12.40624999931720218, 2.654700538379254571 ) ) ;
#1485 = EDGE_CURVE ( 'NONE', #7100, #1707, #10019, .T. ) ;
#1486 = CIRCLE ( 'NONE', #8392, 1.928074011315806136 ) ;
#1487 = CARTESIAN_POINT ( 'NONE',  ( -62.86468353124998032, 14.43229166632526805, 1.000774730468978246 ) ) ;
#1488 = ORIENTED_EDGE ( 'NONE', *, *, #6990, .F. ) ;
#1489 = CARTESIAN_POINT ( 'NONE',  ( -61.99999999999998579, 10.95312499965860020, 0.5015494609379544944 ) ) ;
#1490 = DIRECTION ( 'NONE',  ( -0.000000000000000000, -0.000000000000000000, -1.000000000000000000 ) ) ;
#1491 = VECTOR ( 'NONE', #1699, 1000.000000000000000 ) ;
#1492 = CARTESIAN_POINT ( 'NONE',  ( -61.56765823437498852, 15.59895833299193590, 2.248837904296538515 ) ) ;
#1493 = ORIENTED_EDGE ( 'NONE', *, *, #9866, .F. ) ;
#1494 = CARTESIAN_POINT ( 'NONE',  ( 1.314929834301322591E-16, 0.000000000000000000, 0.000000000000000000 ) ) ;
#1495 = EDGE_CURVE ( 'NONE', #3366, #2273, #2351, .T. ) ;
#1496 = ORIENTED_EDGE ( 'NONE', *, *, #3408, .F. ) ;
#1497 = PLANE ( 'NONE',  #200 ) ;
#1498 = CARTESIAN_POINT ( 'NONE',  ( -60.99999999999998579, 9.229166666666667851, 2.077350269189628840 ) ) ;
#1499 = CARTESIAN_POINT ( 'NONE',  ( -49.99999999999998579, 2.500000000000000000, 4.000000000000000000 ) ) ;
#1500 = DIRECTION ( 'NONE',  ( -0.000000000000000000, -0.000000000000000000, -1.000000000000000000 ) ) ;
#1501 = CARTESIAN_POINT ( 'NONE',  ( -149.9999999999999716, -8.000000000000000000, 3.000000000000000000 ) ) ;
#1502 = DIRECTION ( 'NONE',  ( -0.000000000000000000, -1.000000000000000000, -0.000000000000000000 ) ) ;
#1503 = CARTESIAN_POINT ( 'NONE',  ( -61.99999999999998579, 12.20312499965860198, 0.5015494609379544944 ) ) ;
#1504 = CARTESIAN_POINT ( 'NONE',  ( -62.99999999999998579, 9.114583332650536107, 2.077350269189627952 ) ) ;
#1505 = EDGE_LOOP ( 'NONE', ( #10466, #4149, #3036, #8916 ) ) ;
#1506 = DIRECTION ( 'NONE',  ( 0.000000000000000000, -1.000000000000000000, 0.000000000000000000 ) ) ;
#1507 = ADVANCED_FACE ( 'NONE', ( #8298 ), #740, .F. ) ;
#1508 = ORIENTED_EDGE ( 'NONE', *, *, #1752, .F. ) ;
#1509 = CARTESIAN_POINT ( 'NONE',  ( -114.9999999999999289, -15.00000000000001421, 5.000000000000004441 ) ) ;
#1510 = CARTESIAN_POINT ( 'NONE',  ( -62.43234176562499016, 13.49479166632526805, 2.248837904296538071 ) ) ;
#1511 = DIRECTION ( 'NONE',  ( 0.000000000000000000, 0.000000000000000000, 1.000000000000000000 ) ) ;
#1512 = CARTESIAN_POINT ( 'NONE',  ( -61.99999999999998579, 14.56249999999999822, 0.5000000000000013323 ) ) ;
#1513 = DIRECTION ( 'NONE',  ( -0.000000000000000000, -1.000000000000000000, -0.000000000000000000 ) ) ;
#1514 = CARTESIAN_POINT ( 'NONE',  ( -62.86468353124999453, 12.28645833299193413, 1.999225269531025750 ) ) ;
#1515 = CARTESIAN_POINT ( 'NONE',  ( -62.86468353124998032, 15.99479166632526805, 1.000774730468978246 ) ) ;
#1516 = CARTESIAN_POINT ( 'NONE',  ( -78.99999999999998579, 11.49999999999999645, 8.000000000000000000 ) ) ;
#1517 = CONTEXT_DEPENDENT_SHAPE_REPRESENTATION ( #8911, #8306 ) ;
#1518 = CYLINDRICAL_SURFACE ( 'NONE', #8159, 2.500000000000002220 ) ;
#1519 = ADVANCED_FACE ( 'NONE', ( #639 ), #5792, .F. ) ;
#1520 = CARTESIAN_POINT ( 'NONE',  ( -61.49999999999998579, 15.51041666598387003, 0.6339745962155628467 ) ) ;
#1521 = DIRECTION ( 'NONE',  ( -0.000000000000000000, -1.000000000000000000, -0.000000000000000000 ) ) ;
#1522 = ORIENTED_EDGE ( 'NONE', *, *, #1154, .F. ) ;
#1523 = DIRECTION ( 'NONE',  ( -0.000000000000000000, -1.000000000000000000, -0.000000000000000000 ) ) ;
#1524 = CARTESIAN_POINT ( 'NONE',  ( -61.99999999999998579, 8.062500000000000000, 0.5000000000000013323 ) ) ;
#1525 =( BOUNDED_CURVE ( )  B_SPLINE_CURVE ( 2, ( #7048, #8778, #9543, #4655, #8948, #1158, #8116, #447, #1339 ),
 .UNSPECIFIED., .F., .T. ) 
 B_SPLINE_CURVE_WITH_KNOTS ( ( 3, 2, 2, 2, 3 ),
 ( 0.08593750000000000000, 0.08854166666666667129, 0.09375000000000000000, 0.09895833333333332871, 0.1015624999999999722 ),
 .UNSPECIFIED. ) 
 CURVE ( )  GEOMETRIC_REPRESENTATION_ITEM ( )  RATIONAL_B_SPLINE_CURVE ( ( 0.9330127018922194093, 0.9330127018922194093, 1.000000000000000000, 0.8660254037844387076, 1.000000000000000000, 0.8660254037844387076, 1.000000000000000000, 0.9330127018922200755, 0.9330127018922194093 ) ) 
 REPRESENTATION_ITEM ( '' )  );
#1526 = CARTESIAN_POINT ( 'NONE',  ( -61.13531646874997705, 14.84895833299193413, 1.000774730468978468 ) ) ;
#1527 = CARTESIAN_POINT ( 'NONE',  ( -62.43234176562499016, 9.244791666325268054, 2.248837904296538071 ) ) ;
#1528 = CARTESIAN_POINT ( 'NONE',  ( -62.86468353124999453, 15.78645833299193590, 1.999225269531025750 ) ) ;
#1529 = EDGE_LOOP ( 'NONE', ( #4978, #1374, #5395 ) ) ;
#1530 = CARTESIAN_POINT ( 'NONE',  ( -62.49999999999998579, 14.41666666666666785, 2.366025403784441483 ) ) ;
#1531 = CARTESIAN_POINT ( 'NONE',  ( -61.99999999999998579, 13.65624999931720218, 2.500000000000002665 ) ) ;
#1532 = CARTESIAN_POINT ( 'NONE',  ( -61.49999999999998579, 12.42708333265053611, 2.366025403784441927 ) ) ;
#1533 = CARTESIAN_POINT ( 'NONE',  ( 144.0000000000000284, -5.500000000000000000, 0.000000000000000000 ) ) ;
#1534 = CARTESIAN_POINT ( 'NONE',  ( -62.43234176562499016, 13.49479166632526805, 2.248837904296538071 ) ) ;
#1535 = CARTESIAN_POINT ( 'NONE',  ( -60.99999999999998579, 11.50000000000000000, 1.500000000000002220 ) ) ;
#1536 = ORIENTED_EDGE ( 'NONE', *, *, #5232, .F. ) ;
#1537 = ADVANCED_FACE ( 'NONE', ( #4170 ), #3392, .T. ) ;
#1538 = CARTESIAN_POINT ( 'NONE',  ( -62.86468353124998742, 11.78645833299193590, 1.999225269531025972 ) ) ;
#1539 = DIRECTION ( 'NONE',  ( -0.000000000000000000, -1.000000000000000000, -0.000000000000000000 ) ) ;
#1540 = FACE_OUTER_BOUND ( 'NONE', #2254, .T. ) ;
#1541 = ORIENTED_EDGE ( 'NONE', *, *, #7256, .T. ) ;
#1542 = DIRECTION ( 'NONE',  ( 0.000000000000000000, -1.000000000000000000, 0.000000000000000000 ) ) ;
#1543 = ORIENTED_EDGE ( 'NONE', *, *, #5697, .T. ) ;
#1544 = CARTESIAN_POINT ( 'NONE',  ( -60.99999999999998579, 9.468749999317202182, 1.500000000000002220 ) ) ;
#1545 = CARTESIAN_POINT ( 'NONE',  ( -61.49999999999998579, 11.45833333333333393, 2.366025403784441927 ) ) ;
#1546 = AXIS2_PLACEMENT_3D ( 'NONE', #2475, #10760, #7484 ) ;
#1547 = CARTESIAN_POINT ( 'NONE',  ( -60.99999999999998579, 8.479166666666666075, 2.077350269189628840 ) ) ;
#1548 = CARTESIAN_POINT ( 'NONE',  ( -61.49999999999998579, 12.29166666666666607, 0.6339745962155628467 ) ) ;
#1549 = CARTESIAN_POINT ( 'NONE',  ( -61.99999999999998579, 8.656249999317202182, 2.654700538379254571 ) ) ;
#1550 = EDGE_CURVE ( 'NONE', #3881, #2721, #10065, .T. ) ;
#1551 = CARTESIAN_POINT ( 'NONE',  ( -61.13531646874998415, 11.89062499965860198, 1.500000000000002220 ) ) ;
#1552 = DIRECTION ( 'NONE',  ( 1.000000000000000000, 0.000000000000000000, -0.000000000000000000 ) ) ;
#1553 = ORIENTED_EDGE ( 'NONE', *, *, #8136, .F. ) ;
#1554 = CARTESIAN_POINT ( 'NONE',  ( -61.99999999999998579, 9.156249999317203958, 2.500000000000002665 ) ) ;
#1555 = AXIS2_PLACEMENT_3D ( 'NONE', #10106, #4212, #782 ) ;
#1556 = PRODUCT_DEFINITION_SHAPE ( 'NONE', 'NONE',  #1620 ) ;
#1557 = ORIENTED_EDGE ( 'NONE', *, *, #6848, .T. ) ;
#1558 = DIRECTION ( 'NONE',  ( 1.000000000000000000, 1.224646799147355672E-16, -0.000000000000000000 ) ) ;
#1559 = CARTESIAN_POINT ( 'NONE',  ( -61.56765823437498142, 14.36979166632526983, 0.7511620957034663704 ) ) ;
#1560 = LINE ( 'NONE', #8344, #5022 ) ;
#1561 = CARTESIAN_POINT ( 'NONE',  ( -62.99999999999998579, 8.364583332650536107, 2.077350269189627952 ) ) ;
#1562 = CARTESIAN_POINT ( 'NONE',  ( -61.13531646874998415, 12.14062499965860198, 1.500000000000002220 ) ) ;
#1563 = VECTOR ( 'NONE', #3177, 1000.000000000000000 ) ;
#1564 = CARTESIAN_POINT ( 'NONE',  ( -61.13531646874998415, 8.078124999658601979, 1.500000000000002220 ) ) ;
#1565 = DIRECTION ( 'NONE',  ( 1.000000000000000000, -0.000000000000000000, 0.000000000000000000 ) ) ;
#1566 = CARTESIAN_POINT ( 'NONE',  ( -114.9999999999999289, -15.00000000000001421, 0.000000000000000000 ) ) ;
#1567 = CARTESIAN_POINT ( 'NONE',  ( -62.99999999999998579, 15.36458333265053611, 2.077350269189627952 ) ) ;
#1568 = VECTOR ( 'NONE', #334, 1000.000000000000000 ) ;
#1569 = CARTESIAN_POINT ( 'NONE',  ( -149.9999999999999716, -8.000000000000000000, 3.000000000000000000 ) ) ;
#1570 = ORIENTED_EDGE ( 'NONE', *, *, #9359, .F. ) ;
#1571 = CARTESIAN_POINT ( 'NONE',  ( 3.489067535589073648E-18, 0.000000000000000000, 0.000000000000000000 ) ) ;
#1572 = DIRECTION ( 'NONE',  ( 0.000000000000000000, 0.000000000000000000, 1.000000000000000000 ) ) ;
#1573 = CARTESIAN_POINT ( 'NONE',  ( -61.99999999999999289, 14.01562499965860376, 2.498450539062049724 ) ) ;
#1574 = CARTESIAN_POINT ( 'NONE',  ( -61.13531646874998415, 10.09895833299193413, 1.000774730468978468 ) ) ;
#1575 = CARTESIAN_POINT ( 'NONE',  ( -61.56765823437498852, 15.09895833299193590, 2.248837904296538515 ) ) ;
#1576 = VECTOR ( 'NONE', #6088, 1000.000000000000000 ) ;
#1577 = DIRECTION ( 'NONE',  ( -1.000000000000000000, -3.469446951953572774E-16, 0.000000000000000000 ) ) ;
#1578 = VERTEX_POINT ( 'NONE', #3234 ) ;
#1579 = CARTESIAN_POINT ( 'NONE',  ( -61.49999999999998579, 13.20833333333333215, 2.366025403784441927 ) ) ;
#1580 = CARTESIAN_POINT ( 'NONE',  ( -61.13531646874997705, 9.369791666325268054, 1.999225269531026417 ) ) ;
#1581 = VECTOR ( 'NONE', #4734, 1000.000000000000000 ) ;
#1582 = CARTESIAN_POINT ( 'NONE',  ( -62.99999999999998579, 12.07291666598386826, 0.9226497308103756012 ) ) ;
#1583 = DIRECTION ( 'NONE',  ( -1.000000000000000000, 0.000000000000000000, -0.000000000000000000 ) ) ;
#1584 = COLOUR_RGB ( '',0.8941176470588234615, 0.8941176470588234615, 0.8941176470588234615 ) ;
#1585 =( BOUNDED_CURVE ( )  B_SPLINE_CURVE ( 2, ( #6236, #9729, #281, #3844, #2013, #7234, #5387, #7959, #5563 ),
 .UNSPECIFIED., .F., .F. ) 
 B_SPLINE_CURVE_WITH_KNOTS ( ( 3, 2, 2, 2, 3 ),
 ( 0.5078125000000000000, 0.5104166666666666297, 0.5156250000000000000, 0.5208333333333333703, 0.5234375000000000000 ),
 .UNSPECIFIED. ) 
 CURVE ( )  GEOMETRIC_REPRESENTATION_ITEM ( )  RATIONAL_B_SPLINE_CURVE ( ( 0.9330127018922194093, 0.9330127018922194093, 1.000000000000000000, 0.8660254037844387076, 1.000000000000000000, 0.8660254037844387076, 1.000000000000000000, 0.9330127018922194093, 0.9330127018922194093 ) ) 
 REPRESENTATION_ITEM ( '' )  );
#1586 = CARTESIAN_POINT ( 'NONE',  ( -61.99999999999998579, 14.14062499965860020, 0.5015494609379544944 ) ) ;
#1587 = EDGE_CURVE ( 'NONE', #6091, #7156, #6797, .T. ) ;
#1588 = FILL_AREA_STYLE_COLOUR ( '', #5453 ) ;
#1589 = VECTOR ( 'NONE', #2536, 1000.000000000000000 ) ;
#1590 = ORIENTED_EDGE ( 'NONE', *, *, #8473, .F. ) ;
#1591 = COLOUR_RGB ( '',1.000000000000000000, 0.9490196078431372140, 0.9098039215686274384 ) ;
#1592 = CARTESIAN_POINT ( 'NONE',  ( -61.56765823437498852, 12.59895833299193413, 2.248837904296538515 ) ) ;
#1593 = CARTESIAN_POINT ( 'NONE',  ( -61.99999999999998579, 16.00000000000000000, 1.500000000000002220 ) ) ;
#1594 = AXIS2_PLACEMENT_3D ( 'NONE', #1609, #8605, #4362 ) ;
#1595 = CARTESIAN_POINT ( 'NONE',  ( -114.9999999999999147, -43.00000000000000000, -2.000000000000000000 ) ) ;
#1596 = ORIENTED_EDGE ( 'NONE', *, *, #943, .T. ) ;
#1597 = LINE ( 'NONE', #10875, #4744 ) ;
#1598 = PRODUCT_DEFINITION_FORMATION_WITH_SPECIFIED_SOURCE ( 'ANY', '', #6542, .NOT_KNOWN. ) ;
#1599 = VERTEX_POINT ( 'NONE', #2455 ) ;
#1600 = DIRECTION ( 'NONE',  ( -0.000000000000000000, -0.000000000000000000, -1.000000000000000000 ) ) ;
#1601 = CARTESIAN_POINT ( 'NONE',  ( -62.99999999999998579, 11.14583333333333393, 2.077350269189627952 ) ) ;
#1602 = ORIENTED_EDGE ( 'NONE', *, *, #118, .T. ) ;
#1603 = CARTESIAN_POINT ( 'NONE',  ( -61.49999999999998579, 8.458333333333333925, 2.366025403784441927 ) ) ;
#1604 = CARTESIAN_POINT ( 'NONE',  ( -62.99999999999998579, 15.89583333333333215, 2.077350269189627952 ) ) ;
#1605 = ADVANCED_FACE ( 'NONE', ( #7571 ), #8225, .F. ) ;
#1606 = CARTESIAN_POINT ( 'NONE',  ( -62.43234176562498305, 12.97395833299193590, 0.7511620957034662593 ) ) ;
#1607 = CARTESIAN_POINT ( 'NONE',  ( -62.99999999999998579, 9.072916665983868256, 0.9226497308103756012 ) ) ;
#1608 = VERTEX_POINT ( 'NONE', #5742 ) ;
#1609 = CARTESIAN_POINT ( 'NONE',  ( 145.0000000000000284, 5.500000000000000000, 6.000000000000000000 ) ) ;
#1610 = EDGE_CURVE ( 'NONE', #8468, #3410, #8114, .T. ) ;
#1611 =( BOUNDED_CURVE ( )  B_SPLINE_CURVE ( 2, ( #9651, #9237, #4999, #7208, #10058, #2212, #4164, #1621, #6635 ),
 .UNSPECIFIED., .F., .F. ) 
 B_SPLINE_CURVE_WITH_KNOTS ( ( 3, 2, 2, 2, 3 ),
 ( 0.8671875000000000000, 0.8697916666666666297, 0.8750000000000000000, 0.8802083333333333703, 0.8828125000000000000 ),
 .UNSPECIFIED. ) 
 CURVE ( )  GEOMETRIC_REPRESENTATION_ITEM ( )  RATIONAL_B_SPLINE_CURVE ( ( 0.9330127018922194093, 0.9330127018922194093, 1.000000000000000000, 0.8660254037844387076, 1.000000000000000000, 0.8660254037844387076, 1.000000000000000000, 0.9330127018922194093, 0.9330127018922194093 ) ) 
 REPRESENTATION_ITEM ( '' )  );
#1612 = VERTEX_POINT ( 'NONE', #4125 ) ;
#1613 = DIRECTION ( 'NONE',  ( 0.000000000000000000, 0.000000000000000000, -1.000000000000000000 ) ) ;
#1614 = EDGE_CURVE ( 'NONE', #3158, #10494, #1941, .T. ) ;
#1615 = CARTESIAN_POINT ( 'NONE',  ( -61.13531646874998415, 14.59895833299193590, 1.000774730468978468 ) ) ;
#1616 = DIRECTION ( 'NONE',  ( 0.000000000000000000, 0.000000000000000000, -1.000000000000000000 ) ) ;
#1617 = DIRECTION ( 'NONE',  ( -0.000000000000000000, -1.000000000000000000, -0.000000000000000000 ) ) ;
#1618 = CARTESIAN_POINT ( 'NONE',  ( -62.43234176562499016, 12.55729166632526805, 2.248837904296538071 ) ) ;
#1619 = CARTESIAN_POINT ( 'NONE',  ( -62.43234176562498305, 15.22395833299193590, 0.7511620957034662593 ) ) ;
#1621 = CARTESIAN_POINT ( 'NONE',  ( -61.73205080756886076, 15.05133545031537068, 0.5000000000000014433 ) ) ;
#1620 = PRODUCT_DEFINITION ( 'UNKNOWN', '', #6403, #399 ) ;
#1622 = DIRECTION ( 'NONE',  ( 0.000000000000000000, -0.000000000000000000, -1.000000000000000000 ) ) ;
#1623 = AXIS2_PLACEMENT_3D ( 'NONE', #9057, #2172, #7494 ) ;
#1624 = CARTESIAN_POINT ( 'NONE',  ( -61.13531646874998415, 8.640624999658601979, 1.500000000000002220 ) ) ;
#1625 = PLANE ( 'NONE',  #9971 ) ;
#1626 = EDGE_LOOP ( 'NONE', ( #5551, #6407, #1989, #2000 ) ) ;
#1627 = CARTESIAN_POINT ( 'NONE',  ( -149.9999999999999716, 8.000000000000000000, 3.000000000000000000 ) ) ;
#1628 = CARTESIAN_POINT ( 'NONE',  ( -60.99999999999998579, 8.000000000000000000, 1.500000000000002220 ) ) ;
#1629 = CLOSED_SHELL ( 'NONE', ( #3641, #13, #7424, #7023, #3241, #9816, #9154, #8281, #8359, #2977, #2527, #640, #4769, #7997, #5715, #2128 ) ) ;
#1630 = CARTESIAN_POINT ( 'NONE',  ( -62.43234176562498305, 14.66145833299193413, 0.7511620957034662593 ) ) ;
#1631 = EDGE_CURVE ( 'NONE', #6280, #8297, #4850, .T. ) ;
#1632 = CARTESIAN_POINT ( 'NONE',  ( -61.13531646874998415, 11.57812499965860198, 1.500000000000002220 ) ) ;
#1633 = CARTESIAN_POINT ( 'NONE',  ( -62.86468353124999453, 8.203124999658601979, 1.500000000000002220 ) ) ;
#1634 = CARTESIAN_POINT ( 'NONE',  ( 11.30000000000000426, 0.000000000000000000, 0.000000000000000000 ) ) ;
#1635 = ORIENTED_EDGE ( 'NONE', *, *, #4924, .T. ) ;
#1636 = CARTESIAN_POINT ( 'NONE',  ( -62.49999999999998579, 13.91666666666666785, 2.366025403784441483 ) ) ;
#1637 = CARTESIAN_POINT ( 'NONE',  ( -61.13531646874998415, 8.890624999658601979, 1.500000000000002220 ) ) ;
#1638 =( LENGTH_UNIT ( ) NAMED_UNIT ( * ) SI_UNIT ( .MILLI., .METRE. ) );
#1639 = CARTESIAN_POINT ( 'NONE',  ( -62.49999999999998579, 12.55208333265053611, 0.6339745962155627357 ) ) ;
#1640 = EDGE_LOOP ( 'NONE', ( #7038, #6985, #63, #431, #10351, #8760 ) ) ;
#1641 = CIRCLE ( 'NONE', #3225, 1.000000000000000888 ) ;
#1642 = AXIS2_PLACEMENT_3D ( 'NONE', #9279, #5885, #8442 ) ;
#1643 = SURFACE_STYLE_FILL_AREA ( #4085 ) ;
#1644 = EDGE_CURVE ( 'NONE', #3802, #570, #6077, .T. ) ;
#1645 = CARTESIAN_POINT ( 'NONE',  ( -61.13531646874998415, 13.55729166632526805, 1.999225269531026417 ) ) ;
#1646 =( NAMED_UNIT ( * ) SI_UNIT ( $, .STERADIAN. ) SOLID_ANGLE_UNIT ( ) );
#1647 = EDGE_CURVE ( 'NONE', #10509, #1800, #87, .T. ) ;
#1648 = VERTEX_POINT ( 'NONE', #5161 ) ;
#1649 = AXIS2_PLACEMENT_3D ( 'NONE', #791, #6592, #7472 ) ;
#1650 = AXIS2_PLACEMENT_3D ( 'NONE', #595, #643, #7419 ) ;
#1651 = CARTESIAN_POINT ( 'NONE',  ( -62.86468353124999453, 13.51562499965860020, 1.500000000000002220 ) ) ;
#1652 = DIRECTION ( 'NONE',  ( 0.000000000000000000, 0.000000000000000000, 1.000000000000000000 ) ) ;
#1653 = ADVANCED_FACE ( 'NONE', ( #2736 ), #8678, .T. ) ;
#1654 = CARTESIAN_POINT ( 'NONE',  ( 0.000000000000000000, -0.2499999999999997780, -2.000000000000000000 ) ) ;
#1655 = ORIENTED_EDGE ( 'NONE', *, *, #8885, .T. ) ;
#1656 = VECTOR ( 'NONE', #9806, 1000.000000000000000 ) ;
#1657 = CARTESIAN_POINT ( 'NONE',  ( -49.99998799999998766, -10.00000000000000888, 3.141811147483251965 ) ) ;
#1658 = ORIENTED_EDGE ( 'NONE', *, *, #4363, .T. ) ;
#1659 = CARTESIAN_POINT ( 'NONE',  ( -60.99999999999998579, 11.25000000000000000, 1.500000000000002220 ) ) ;
#1661 = EDGE_LOOP ( 'NONE', ( #7893, #2024, #4379, #10621 ) ) ;
#1660 = APPLICATION_CONTEXT ( 'automotive_design' ) ;
#1662 = CARTESIAN_POINT ( 'NONE',  ( -62.86468353124999453, 9.515624999658600203, 1.500000000000002220 ) ) ;
#1663 = FACE_OUTER_BOUND ( 'NONE', #6726, .T. ) ;
#1664 = VECTOR ( 'NONE', #4606, 1000.000000000000000 ) ;
#1665 = CARTESIAN_POINT ( 'NONE',  ( -62.43234176562499016, 13.30729166632526805, 2.248837904296538071 ) ) ;
#1666 = CARTESIAN_POINT ( 'NONE',  ( -61.99999999999998579, 13.31249999999999822, 0.5000000000000013323 ) ) ;
#1667 = ORIENTED_EDGE ( 'NONE', *, *, #3852, .T. ) ;
#1668 = LINE ( 'NONE', #7665, #7103 ) ;
#1669 = ORIENTED_EDGE ( 'NONE', *, *, #5664, .F. ) ;
#1670 = CARTESIAN_POINT ( 'NONE',  ( -61.99999999999998579, 9.937500000000000000, 2.500000000000002665 ) ) ;
#1671 = EDGE_CURVE ( 'NONE', #427, #10197, #5953, .T. ) ;
#1672 = CARTESIAN_POINT ( 'NONE',  ( -62.86468353124999453, 14.95312499965860020, 1.500000000000002220 ) ) ;
#1673 = CARTESIAN_POINT ( 'NONE',  ( -62.49999999999998579, 11.91666666666666607, 2.366025403784441483 ) ) ;
#1674 = CARTESIAN_POINT ( 'NONE',  ( 0.000000000000000000, 2.310008073021392480E-16, 1.886264737416298409 ) ) ;
#1675 = CARTESIAN_POINT ( 'NONE',  ( -61.99999999999998579, 10.81250000000000000, 0.5000000000000013323 ) ) ;
#1676 = CARTESIAN_POINT ( 'NONE',  ( -62.43234176562499016, 13.30729166632526805, 2.248837904296538071 ) ) ;
#1677 = CARTESIAN_POINT ( 'NONE',  ( -61.13531646874998415, 15.11979166632526628, 1.999225269531026417 ) ) ;
#1678 = ADVANCED_FACE ( 'NONE', ( #1731 ), #3448, .F. ) ;
#1679 = CARTESIAN_POINT ( 'NONE',  ( -60.99999999999998579, 9.270833333333333925, 0.9226497308103762673 ) ) ;
#1680 = CARTESIAN_POINT ( 'NONE',  ( -62.86468353124998032, 9.244791666325268054, 1.000774730468978246 ) ) ;
#1681 = CARTESIAN_POINT ( 'NONE',  ( -62.99999999999998579, 10.37500000000000000, 1.500000000000001998 ) ) ;
#1682 = EDGE_LOOP ( 'NONE', ( #6021, #5235, #10747, #9316 ) ) ;
#1683 = PLANE ( 'NONE',  #2131 ) ;
#1684 = CARTESIAN_POINT ( 'NONE',  ( 0.5000000000000000000, 0.2499999999999998335, -1.911797424705720116 ) ) ;
#1685 = CARTESIAN_POINT ( 'NONE',  ( -62.86468353124999453, 14.97395833299193590, 1.999225269531025750 ) ) ;
#1686 = CARTESIAN_POINT ( 'NONE',  ( -61.13531646874998415, 10.80729166632526628, 1.999225269531026417 ) ) ;
#1687 = CARTESIAN_POINT ( 'NONE',  ( -62.86468353124998032, 15.49479166632526628, 1.000774730468978024 ) ) ;
#1688 = CARTESIAN_POINT ( 'NONE',  ( 146.0000000000000284, 5.500000000000000000, 0.000000000000000000 ) ) ;
#1689 = EDGE_LOOP ( 'NONE', ( #1390, #4553, #3987, #4068 ) ) ;
#1690 = CARTESIAN_POINT ( 'NONE',  ( -60.99999999999998579, 14.97916666666666785, 2.077350269189628840 ) ) ;
#1691 = CARTESIAN_POINT ( 'NONE',  ( -61.99999999999999289, 9.078124999658601979, 2.498450539062049724 ) ) ;
#1692 = CARTESIAN_POINT ( 'NONE',  ( -62.99999999999998579, 13.86458333265053611, 2.077350269189627952 ) ) ;
#1693 = EDGE_LOOP ( 'NONE', ( #9838, #1184 ) ) ;
#1694 = EDGE_CURVE ( 'NONE', #1612, #1296, #8738, .T. ) ;
#1695 = FACE_OUTER_BOUND ( 'NONE', #6216, .T. ) ;
#1696 = CARTESIAN_POINT ( 'NONE',  ( -61.99999999999998579, 14.26562499965860020, 2.498450539062049724 ) ) ;
#1697 = DIRECTION ( 'NONE',  ( -0.000000000000000000, -0.000000000000000000, 1.000000000000000000 ) ) ;
#1698 = VERTEX_POINT ( 'NONE', #8512 ) ;
#1699 = DIRECTION ( 'NONE',  ( -0.000000000000000000, -1.000000000000000000, -0.000000000000000000 ) ) ;
#1700 = CARTESIAN_POINT ( 'NONE',  ( -61.56765823437498852, 13.09895833299193413, 2.248837904296538515 ) ) ;
#1701 = FACE_OUTER_BOUND ( 'NONE', #4474, .T. ) ;
#1702 = VERTEX_POINT ( 'NONE', #6904 ) ;
#1703 = LINE ( 'NONE', #34, #9038 ) ;
#1704 = ORIENTED_EDGE ( 'NONE', *, *, #473, .T. ) ;
#1705 = DIRECTION ( 'NONE',  ( 1.000000000000000000, 0.000000000000000000, 0.000000000000000000 ) ) ;
#1706 = DIRECTION ( 'NONE',  ( 1.000000000000000000, 0.000000000000000000, 0.000000000000000000 ) ) ;
#1707 = VERTEX_POINT ( 'NONE', #949 ) ;
#1708 = ADVANCED_FACE ( 'NONE', ( #1000 ), #1900, .T. ) ;
#1709 = ORIENTED_EDGE ( 'NONE', *, *, #3265, .T. ) ;
#1710 = CARTESIAN_POINT ( 'NONE',  ( -61.13531646874998415, 8.911458332991934128, 1.000774730468978468 ) ) ;
#1711 = CARTESIAN_POINT ( 'NONE',  ( 0.5000000000000000000, -0.2499999999999997780, -1.911797424705720116 ) ) ;
#1712 = CARTESIAN_POINT ( 'NONE',  ( -61.99999999999998579, 12.82812499965860198, 2.498450539062049724 ) ) ;
#1713 = CARTESIAN_POINT ( 'NONE',  ( 143.9000000000000341, -5.500000000000000000, 6.000000000000000000 ) ) ;
#1714 = VERTEX_POINT ( 'NONE', #2682 ) ;
#1715 = DIRECTION ( 'NONE',  ( -1.110223024625156343E-15, 1.000000000000000000, 0.000000000000000000 ) ) ;
#1716 = ORIENTED_EDGE ( 'NONE', *, *, #3494, .T. ) ;
#1717 = LINE ( 'NONE', #6106, #5354 ) ;
#1718 = EDGE_CURVE ( 'NONE', #7701, #9934, #9836, .T. ) ;
#1719 = CARTESIAN_POINT ( 'NONE',  ( -62.43234176562498305, 15.16145833299193590, 0.7511620957034662593 ) ) ;
#1720 = CARTESIAN_POINT ( 'NONE',  ( -61.49999999999998579, 13.70833333333333215, 2.366025403784441927 ) ) ;
#1721 = CARTESIAN_POINT ( 'NONE',  ( -61.73205080756886076, 12.41741454900183150, 2.500000000000003109 ) ) ;
#1722 = DIRECTION ( 'NONE',  ( -0.000000000000000000, -1.000000000000000000, -0.000000000000000000 ) ) ;
#1723 = CARTESIAN_POINT ( 'NONE',  ( -61.13531646874997705, 12.66145833299193413, 1.000774730468978468 ) ) ;
#1724 = CARTESIAN_POINT ( 'NONE',  ( -62.86468353124999453, 8.703124999658601979, 1.500000000000002220 ) ) ;
#1725 = LINE ( 'NONE', #6950, #10974 ) ;
#1726 = CARTESIAN_POINT ( 'NONE',  ( 7.300000000000000711, 1.224646799147353207E-16, -1.000000000000000000 ) ) ;
#1727 = CARTESIAN_POINT ( 'NONE',  ( -62.86468353124998032, 8.744791666325268054, 1.000774730468978246 ) ) ;
#1728 = CARTESIAN_POINT ( 'NONE',  ( -37.99999999999999289, -14.00000000000000888, -2.000000000000000000 ) ) ;
#1729 = ORIENTED_EDGE ( 'NONE', *, *, #4171, .T. ) ;
#1730 = LINE ( 'NONE', #6063, #2660 ) ;
#1731 = FACE_OUTER_BOUND ( 'NONE', #7420, .T. ) ;
#1732 = EDGE_CURVE ( 'NONE', #1268, #9081, #3088, .T. ) ;
#1733 = CARTESIAN_POINT ( 'NONE',  ( -62.43234176562499016, 15.99479166632526628, 2.248837904296538071 ) ) ;
#1734 = EDGE_CURVE ( 'NONE', #6626, #1104, #4194, .T. ) ;
#1735 = CARTESIAN_POINT ( 'NONE',  ( -62.86468353124999453, 10.70312499965860020, 1.500000000000002220 ) ) ;
#1736 = AXIS2_PLACEMENT_3D ( 'NONE', #10398, #354, #10574 ) ;
#1737 = CARTESIAN_POINT ( 'NONE',  ( -62.86468353124999453, 15.51562499965860198, 1.500000000000002220 ) ) ;
#1738 = DIRECTION ( 'NONE',  ( 0.000000000000000000, 0.000000000000000000, 1.000000000000000000 ) ) ;
#1739 = ORIENTED_EDGE ( 'NONE', *, *, #7365, .F. ) ;
#1740 = CARTESIAN_POINT ( 'NONE',  ( -62.99999999999998579, 15.37500000000000000, 1.500000000000001998 ) ) ;
#1741 = PRODUCT_DEFINITION_SHAPE ( 'NONE', 'NONE',  #10982 ) ;
#1742 = CARTESIAN_POINT ( 'NONE',  ( -61.13531646874997705, 9.161458332991935904, 1.000774730468978468 ) ) ;
#1743 = SURFACE_STYLE_USAGE ( .BOTH. , #5225 ) ;
#1744 = CARTESIAN_POINT ( 'NONE',  ( -61.99999999999998579, 13.03124999931720396, 0.3452994616207497591 ) ) ;
#1745 = FACE_OUTER_BOUND ( 'NONE', #9362, .T. ) ;
#1746 =( BOUNDED_CURVE ( )  B_SPLINE_CURVE ( 2, ( #8611, #4210, #6836, #938, #5096, #990, #6109, #1778, #2555 ),
 .UNSPECIFIED., .F., .T. ) 
 B_SPLINE_CURVE_WITH_KNOTS ( ( 3, 2, 2, 2, 3 ),
 ( 0.5546875000000000000, 0.5572916666666666297, 0.5625000000000000000, 0.5677083333333333703, 0.5703125000000000000 ),
 .UNSPECIFIED. ) 
 CURVE ( )  GEOMETRIC_REPRESENTATION_ITEM ( )  RATIONAL_B_SPLINE_CURVE ( ( 0.9330127018922194093, 0.9330127018922194093, 1.000000000000000000, 0.8660254037844387076, 1.000000000000000000, 0.8660254037844387076, 1.000000000000000000, 0.9330127018922194093, 0.9330127018922194093 ) ) 
 REPRESENTATION_ITEM ( '' )  );
#1747 = PRESENTATION_STYLE_ASSIGNMENT (( #7641 ) ) ;
#1748 = EDGE_CURVE ( 'NONE', #570, #3802, #2899, .T. ) ;
#1749 = CARTESIAN_POINT ( 'NONE',  ( -61.99999999999999289, 10.89062499965859843, 0.5015494609379544944 ) ) ;
#1750 = CYLINDRICAL_SURFACE ( 'NONE', #8142, 0.9999999999999981126 ) ;
#1751 = ORIENTED_EDGE ( 'NONE', *, *, #1280, .F. ) ;
#1752 = EDGE_CURVE ( 'NONE', #1136, #10538, #8935, .T. ) ;
#1753 = LINE ( 'NONE', #4344, #8240 ) ;
#1754 = CARTESIAN_POINT ( 'NONE',  ( -62.86468353124998032, 13.24479166632526983, 1.000774730468978246 ) ) ;
#1755 = SURFACE_SIDE_STYLE ('',( #5970 ) ) ;
#1756 = LINE ( 'NONE', #7648, #5474 ) ;
#1757 = CARTESIAN_POINT ( 'NONE',  ( -61.99999999999998579, 9.781249999317202182, 0.3452994616207497591 ) ) ;
#1758 = VECTOR ( 'NONE', #994, 1000.000000000000000 ) ;
#1759 = ORIENTED_EDGE ( 'NONE', *, *, #4363, .F. ) ;
#1760 = DIRECTION ( 'NONE',  ( -0.000000000000000000, -0.000000000000000000, 1.000000000000000000 ) ) ;
#1761 = EDGE_LOOP ( 'NONE', ( #3314, #6943, #1013, #10573 ) ) ;
#1762 = DIRECTION ( 'NONE',  ( -0.000000000000000000, -1.000000000000000000, -0.000000000000000000 ) ) ;
#1763 = AXIS2_PLACEMENT_3D ( 'NONE', #7594, #7880, #6092 ) ;
#1764 = CARTESIAN_POINT ( 'NONE',  ( -61.56765823437498142, 11.86979166632526805, 0.7511620957034663704 ) ) ;
#1765 = STYLED_ITEM ( 'NONE', ( #1145 ), #5753 ) ;
#1766 = ORIENTED_EDGE ( 'NONE', *, *, #9423, .F. ) ;
#1767 = CARTESIAN_POINT ( 'NONE',  ( -61.56765823437498142, 8.682291666325268054, 0.7511620957034663704 ) ) ;
#1768 = CARTESIAN_POINT ( 'NONE',  ( -61.73205080756886076, 14.30133545031537068, 0.5000000000000014433 ) ) ;
#1769 = ITEM_DEFINED_TRANSFORMATION ( 'NONE', 'NONE', #549,  #2307 ) ;
#1770 = CARTESIAN_POINT ( 'NONE',  ( -62.86468353124998742, 12.78645833299193413, 1.999225269531025972 ) ) ;
#1771 = DIRECTION ( 'NONE',  ( -1.000000000000000000, -0.000000000000000000, -0.000000000000000000 ) ) ;
#1772 = ORIENTED_EDGE ( 'NONE', *, *, #2448, .F. ) ;
#1773 = CARTESIAN_POINT ( 'NONE',  ( -61.99999999999998579, 16.00000000000000000, 2.500000000000000444 ) ) ;
#1774 = EDGE_LOOP ( 'NONE', ( #7389, #6028, #6329, #3980 ) ) ;
#1775 = CARTESIAN_POINT ( 'NONE',  ( -61.73205080756886076, 12.80133545031537068, 0.5000000000000014433 ) ) ;
#1776 = CARTESIAN_POINT ( 'NONE',  ( -61.56765823437498852, 15.53645833299193590, 2.248837904296538515 ) ) ;
#1777 = DIRECTION ( 'NONE',  ( 1.000000000000000000, 0.000000000000000000, 0.000000000000000000 ) ) ;
#1778 = CARTESIAN_POINT ( 'NONE',  ( -61.73205080756886076, 12.55133545031537068, 0.5000000000000014433 ) ) ;
#1779 = EDGE_CURVE ( 'NONE', #5869, #2164, #8054, .T. ) ;
#1780 = CARTESIAN_POINT ( 'NONE',  ( -105.0000000000000000, 2.500000000000000000, 4.000000000000000000 ) ) ;
#1781 = CARTESIAN_POINT ( 'NONE',  ( -62.43234176562498305, 13.97395833299193413, 0.7511620957034662593 ) ) ;
#1782 = CARTESIAN_POINT ( 'NONE',  ( -62.86468353124998742, 9.223958332991935904, 1.999225269531025972 ) ) ;
#1783 = CYLINDRICAL_SURFACE ( 'NONE', #3519, 0.9999999999999981126 ) ;
#1784 = CARTESIAN_POINT ( 'NONE',  ( -61.73205080756886076, 13.52008544963257286, 0.5000000000000014433 ) ) ;
#1785 = CARTESIAN_POINT ( 'NONE',  ( -61.13531646874998415, 8.869791666325268054, 1.999225269531026417 ) ) ;
#1786 = CARTESIAN_POINT ( 'NONE',  ( -61.73205080756886076, 15.77008544963257108, 0.5000000000000014433 ) ) ;
#1787 = ORIENTED_EDGE ( 'NONE', *, *, #2951, .T. ) ;
#1788 = LINE ( 'NONE', #4220, #2469 ) ;
#1789 = EDGE_CURVE ( 'NONE', #1800, #562, #3017, .T. ) ;
#1790 = CARTESIAN_POINT ( 'NONE',  ( -61.99999999999998579, 14.99999999999998579, 1.500000000000002220 ) ) ;
#1791 = CARTESIAN_POINT ( 'NONE',  ( -62.86468353124999453, 15.72395833299193590, 1.999225269531025750 ) ) ;
#1792 = CARTESIAN_POINT ( 'NONE',  ( -62.86468353124998032, 10.68229166632526628, 1.000774730468978246 ) ) ;
#1793 = CARTESIAN_POINT ( 'NONE',  ( -62.43234176562498305, 8.911458332991934128, 0.7511620957034662593 ) ) ;
#1794 = FACE_OUTER_BOUND ( 'NONE', #534, .T. ) ;
#1795 = ORIENTED_EDGE ( 'NONE', *, *, #792, .F. ) ;
#1796 = CARTESIAN_POINT ( 'NONE',  ( -61.99999999999998579, 14.43750000000000000, 2.654700538379254571 ) ) ;
#1797 = CARTESIAN_POINT ( 'NONE',  ( -62.86468353124998032, 8.744791666325268054, 1.000774730468978024 ) ) ;
#1798 = CARTESIAN_POINT ( 'NONE',  ( -62.99999999999998579, 13.82291666598387003, 0.9226497308103756012 ) ) ;
#1799 = CARTESIAN_POINT ( 'NONE',  ( -46.99999999999998579, -15.00000000000001066, 3.000000000000000000 ) ) ;
#1800 = VERTEX_POINT ( 'NONE', #2187 ) ;
#1801 = CARTESIAN_POINT ( 'NONE',  ( -61.49999999999998579, 9.708333333333332149, 2.366025403784441927 ) ) ;
#1802 = VECTOR ( 'NONE', #3290, 1000.000000000000000 ) ;
#1803 = CARTESIAN_POINT ( 'NONE',  ( -61.13531646874997705, 11.84895833299193413, 1.000774730468978468 ) ) ;
#1804 =( LENGTH_UNIT ( ) NAMED_UNIT ( * ) SI_UNIT ( .MILLI., .METRE. ) );
#1805 = DIRECTION ( 'NONE',  ( 0.000000000000000000, 0.000000000000000000, 1.000000000000000000 ) ) ;
#1806 = ORIENTED_EDGE ( 'NONE', *, *, #7042, .F. ) ;
#1807 = EDGE_CURVE ( 'NONE', #24, #8835, #9112, .T. ) ;
#1808 = CARTESIAN_POINT ( 'NONE',  ( -42.47213595499957961, -18.00000000000001066, 3.000000000000000000 ) ) ;
#1809 = CARTESIAN_POINT ( 'NONE',  ( -62.86468353124998742, 13.03645833299193235, 1.999225269531025972 ) ) ;
#1810 =( BOUNDED_CURVE ( )  B_SPLINE_CURVE ( 2, ( #3263, #3367, #815, #919, #8596, #5976, #7710, #6663, #3476 ),
 .UNSPECIFIED., .F., .T. ) 
 B_SPLINE_CURVE_WITH_KNOTS ( ( 3, 2, 2, 2, 3 ),
 ( 0.8359375000000000000, 0.8385416666666666297, 0.8437500000000000000, 0.8489583333333333703, 0.8515625000000000000 ),
 .UNSPECIFIED. ) 
 CURVE ( )  GEOMETRIC_REPRESENTATION_ITEM ( )  RATIONAL_B_SPLINE_CURVE ( ( 0.9330127018922194093, 0.9330127018922194093, 1.000000000000000000, 0.8660254037844387076, 1.000000000000000000, 0.8660254037844387076, 1.000000000000000000, 0.9330127018922194093, 0.9330127018922194093 ) ) 
 REPRESENTATION_ITEM ( '' )  );
#1811 = CARTESIAN_POINT ( 'NONE',  ( -61.73205080756886076, 10.19866454968463110, 2.500000000000003109 ) ) ;
#1812 = CIRCLE ( 'NONE', #7492, 1.000000000000000888 ) ;
#1813 = CARTESIAN_POINT ( 'NONE',  ( -61.99999999999998579, 8.906249999317203958, 2.654700538379254571 ) ) ;
#1814 = ADVANCED_FACE ( 'NONE', ( #1356, #408 ), #3904, .F. ) ;
#1815 = ORIENTED_EDGE ( 'NONE', *, *, #7660, .F. ) ;
#1816 = DIRECTION ( 'NONE',  ( -0.000000000000000000, -0.000000000000000000, 1.000000000000000000 ) ) ;
#1817 = ORIENTED_EDGE ( 'NONE', *, *, #5195, .T. ) ;
#1818 = DIRECTION ( 'NONE',  ( -0.000000000000000000, -1.000000000000000000, -0.000000000000000000 ) ) ;
#1819 = VECTOR ( 'NONE', #10581, 1000.000000000000000 ) ;
#1820 = CARTESIAN_POINT ( 'NONE',  ( -62.86468353124999453, 11.95312499965860198, 1.500000000000002220 ) ) ;
#1821 = CONICAL_SURFACE ( 'NONE', #7325, 1.886264737416298409, 0.08726646259971679309 ) ;
#1822 = ORIENTED_EDGE ( 'NONE', *, *, #9409, .T. ) ;
#1823 = CARTESIAN_POINT ( 'NONE',  ( -61.13531646874998415, 9.161458332991935904, 1.000774730468978468 ) ) ;
#1824 = CARTESIAN_POINT ( 'NONE',  ( -105.0000000000000000, -2.500000000000000000, 4.000000000000000000 ) ) ;
#1825 = VECTOR ( 'NONE', #4554, 1000.000000000000000 ) ;
#1826 = CARTESIAN_POINT ( 'NONE',  ( -62.86468353124999453, 13.51562499965860020, 1.500000000000002220 ) ) ;
#1827 = LINE ( 'NONE', #5200, #3582 ) ;
#1828 = ORIENTED_EDGE ( 'NONE', *, *, #10681, .F. ) ;
#1829 = CARTESIAN_POINT ( 'NONE',  ( -114.9999999999999289, -7.999999999999998224, 5.000000000000004441 ) ) ;
#1830 = ADVANCED_FACE ( 'NONE', ( #9009 ), #10511, .T. ) ;
#1831 = PRODUCT_DEFINITION_SHAPE ( 'NONE', 'NONE',  #3118 ) ;
#1832 = ORIENTED_EDGE ( 'NONE', *, *, #8649, .T. ) ;
#1833 = AXIS2_PLACEMENT_3D ( 'NONE', #6481, #6309, #4794 ) ;
#1834 = CARTESIAN_POINT ( 'NONE',  ( -61.49999999999998579, 13.26041666598387003, 0.6339745962155628467 ) ) ;
#1835 = CARTESIAN_POINT ( 'NONE',  ( -61.13531646874998415, 14.80729166632526805, 1.999225269531026417 ) ) ;
#1836 = CARTESIAN_POINT ( 'NONE',  ( -62.99999999999998579, 9.875000000000000000, 1.500000000000001998 ) ) ;
#1837 = LINE ( 'NONE', #9282, #10249 ) ;
#1838 = LINE ( 'NONE', #8612, #6358 ) ;
#1839 = CARTESIAN_POINT ( 'NONE',  ( -62.86468353124998032, 13.99479166632526983, 1.000774730468978024 ) ) ;
#1840 = CARTESIAN_POINT ( 'NONE',  ( -61.99999999999998579, 9.015624999658603755, 2.498450539062049724 ) ) ;
#1841 = CARTESIAN_POINT ( 'NONE',  ( -61.99999999999998579, 16.00000000000000000, 1.500000000000002220 ) ) ;
#1842 = CARTESIAN_POINT ( 'NONE',  ( -105.0000000000000000, -2.500000000000000000, 2.000000000000000000 ) ) ;
#1843 = CARTESIAN_POINT ( 'NONE',  ( -61.56765823437498142, 9.432291666325268054, 0.7511620957034663704 ) ) ;
#1844 = CARTESIAN_POINT ( 'NONE',  ( 0.2300425840023382074, 0.2499999999999982236, -1.812072026511089229 ) ) ;
#1845 = VERTEX_POINT ( 'NONE', #8186 ) ;
#1846 = CARTESIAN_POINT ( 'NONE',  ( 146.0999999999999943, -5.500000000000000000, 6.000000000000000000 ) ) ;
#1847 = CARTESIAN_POINT ( 'NONE',  ( -62.99999999999998579, 11.37500000000000000, 1.500000000000001998 ) ) ;
#1848 = EDGE_CURVE ( 'NONE', #7344, #9337, #10951, .T. ) ;
#1849 = CARTESIAN_POINT ( 'NONE',  ( -61.13531646874997705, 15.09895833299193590, 1.000774730468978468 ) ) ;
#1850 = CARTESIAN_POINT ( 'NONE',  ( -61.56765823437498142, 11.36979166632526805, 0.7511620957034663704 ) ) ;
#1851 = CARTESIAN_POINT ( 'NONE',  ( -62.86468353124999453, 8.973958332991934128, 1.999225269531025750 ) ) ;
#1852 = CARTESIAN_POINT ( 'NONE',  ( -120.0000000000000000, -8.000000000000000000, -2.000000000000000000 ) ) ;
#1853 = ORIENTED_EDGE ( 'NONE', *, *, #6704, .T. ) ;
#1854 = CARTESIAN_POINT ( 'NONE',  ( -61.99999999999998579, 15.18750000000000000, 2.654700538379254571 ) ) ;
#1855 = EDGE_CURVE ( 'NONE', #9209, #7667, #1091, .T. ) ;
#1856 = CARTESIAN_POINT ( 'NONE',  ( -61.13531646874997705, 10.16145833299193413, 1.000774730468978468 ) ) ;
#1857 = CARTESIAN_POINT ( 'NONE',  ( -62.49999999999998579, 13.05208333265053611, 0.6339745962155627357 ) ) ;
#1858 = CARTESIAN_POINT ( 'NONE',  ( 144.0000000000000284, 5.500000000000000000, 3.000000000000000000 ) ) ;
#1859 = ORIENTED_EDGE ( 'NONE', *, *, #4382, .F. ) ;
#1860 = DIRECTION ( 'NONE',  ( -0.000000000000000000, -1.000000000000000000, -0.000000000000000000 ) ) ;
#1861 = CARTESIAN_POINT ( 'NONE',  ( -61.13531646874998415, 11.07812499965860020, 1.500000000000002220 ) ) ;
#1862 = DIRECTION ( 'NONE',  ( -0.000000000000000000, -1.000000000000000000, -0.000000000000000000 ) ) ;
#1863 = DIRECTION ( 'NONE',  ( 0.000000000000000000, 1.000000000000000000, 0.000000000000000000 ) ) ;
#1864 = ORIENTED_EDGE ( 'NONE', *, *, #5528, .T. ) ;
#1865 = CARTESIAN_POINT ( 'NONE',  ( -62.49999999999998579, 10.66666666666666607, 2.366025403784441483 ) ) ;
#1866 = CARTESIAN_POINT ( 'NONE',  ( -49.99999999999998579, -18.00000000000001066, 3.000000000000000000 ) ) ;
#1867 = CARTESIAN_POINT ( 'NONE',  ( -61.56765823437498852, 14.34895833299193413, 2.248837904296538515 ) ) ;
#1868 = FILL_AREA_STYLE_COLOUR ( '', #6571 ) ;
#1869 = CARTESIAN_POINT ( 'NONE',  ( -61.73205080756886076, 10.94866454968462932, 2.500000000000003109 ) ) ;
#1870 = CARTESIAN_POINT ( 'NONE',  ( -60.99999999999998579, 9.468749999317202182, 1.500000000000002220 ) ) ;
#1871 = ORIENTED_EDGE ( 'NONE', *, *, #5613, .T. ) ;
#1872 = LINE ( 'NONE', #5243, #5665 ) ;
#1873 = APPLICATION_CONTEXT ( 'automotive_design' ) ;
#1874 = CARTESIAN_POINT ( 'NONE',  ( -105.0000000000000000, -2.500000000000000000, 4.000000000000000000 ) ) ;
#1875 = CARTESIAN_POINT ( 'NONE',  ( -61.13531646874998415, 11.07812499965860020, 1.500000000000002220 ) ) ;
#1876 = SURFACE_STYLE_USAGE ( .BOTH. , #10308 ) ;
#1877 = EDGE_CURVE ( 'NONE', #1648, #10538, #7962, .T. ) ;
#1878 =( BOUNDED_CURVE ( )  B_SPLINE_CURVE ( 2, ( #5392, #411, #5509, #8913, #1301, #4676, #3850, #6414, #2190 ),
 .UNSPECIFIED., .F., .T. ) 
 B_SPLINE_CURVE_WITH_KNOTS ( ( 3, 2, 2, 2, 3 ),
 ( 0.2421874999999999722, 0.2447916666666666574, 0.2500000000000000000, 0.2552083333333333148, 0.2578125000000000000 ),
 .UNSPECIFIED. ) 
 CURVE ( )  GEOMETRIC_REPRESENTATION_ITEM ( )  RATIONAL_B_SPLINE_CURVE ( ( 0.9330127018922194093, 0.9330127018922186322, 1.000000000000000000, 0.8660254037844387076, 1.000000000000000000, 0.8660254037844387076, 1.000000000000000000, 0.9330127018922194093, 0.9330127018922194093 ) ) 
 REPRESENTATION_ITEM ( '' )  );
#1879 = VERTEX_POINT ( 'NONE', #8083 ) ;
#1880 = CARTESIAN_POINT ( 'NONE',  ( -61.13531646874998415, 9.140624999658601979, 1.500000000000002220 ) ) ;
#1881 = FACE_OUTER_BOUND ( 'NONE', #4804, .T. ) ;
#1882 = CARTESIAN_POINT ( 'NONE',  ( -61.99999999999998579, 15.07812499965860198, 2.498450539062049724 ) ) ;
#1883 = CARTESIAN_POINT ( 'NONE',  ( -60.99999999999998579, 13.25000000000000000, 1.500000000000002220 ) ) ;
#1884 = ORIENTED_EDGE ( 'NONE', *, *, #4763, .F. ) ;
#1885 = CARTESIAN_POINT ( 'NONE',  ( -61.99999999999998579, 16.00000000000000000, 0.5000000000000041078 ) ) ;
#1886 = EDGE_LOOP ( 'NONE', ( #1411, #9822 ) ) ;
#1887 = CARTESIAN_POINT ( 'NONE',  ( -61.99999999999998579, 8.062500000000000000, 0.3452994616207497591 ) ) ;
#1888 = CARTESIAN_POINT ( 'NONE',  ( -49.99998799999998766, -14.00000000000001243, -0.1418111474832477736 ) ) ;
#1889 = CARTESIAN_POINT ( 'NONE',  ( -144.9999999999999716, 33.00000000000000000, 0.000000000000000000 ) ) ;
#1890 = CARTESIAN_POINT ( 'NONE',  ( -61.99999999999997868, 10.65624999931720218, 2.500000000000002665 ) ) ;
#1891 = CARTESIAN_POINT ( 'NONE',  ( -61.13531646874997705, 13.66145833299193413, 1.000774730468978468 ) ) ;
#1892 = EDGE_CURVE ( 'NONE', #10833, #10050, #5506, .T. ) ;
#1893 = CARTESIAN_POINT ( 'NONE',  ( -61.13531646874998415, 8.557291666325268054, 1.999225269531026417 ) ) ;
#1894 = DIRECTION ( 'NONE',  ( -0.000000000000000000, -1.000000000000000000, -0.000000000000000000 ) ) ;
#1895 = CARTESIAN_POINT ( 'NONE',  ( 0.2309188673393136881, 0.2499999999999998890, 1.812888087824517491 ) ) ;
#1896 = CARTESIAN_POINT ( 'NONE',  ( -61.56765823437498852, 9.848958332991934128, 2.248837904296538515 ) ) ;
#1897 = CARTESIAN_POINT ( 'NONE',  ( 0.5000000000000000000, 0.2499999999999982792, -1.911797424705720339 ) ) ;
#1898 = ORIENTED_EDGE ( 'NONE', *, *, #3692, .T. ) ;
#1899 = CARTESIAN_POINT ( 'NONE',  ( -61.99999999999998579, 10.15624999931720041, 2.500000000000002665 ) ) ;
#1900 = CYLINDRICAL_SURFACE ( 'NONE', #44, 0.9999999999999981126 ) ;
#1901 = CARTESIAN_POINT ( 'NONE',  ( -62.86468353124999453, 15.95312499965860198, 1.500000000000002220 ) ) ;
#1902 = CARTESIAN_POINT ( 'NONE',  ( -62.86468353124998032, 12.18229166632526805, 1.000774730468978246 ) ) ;
#1903 = CARTESIAN_POINT ( 'NONE',  ( -62.86468353124999453, 9.203124999658600203, 1.500000000000002220 ) ) ;
#1904 = PRESENTATION_STYLE_ASSIGNMENT (( #8684 ) ) ;
#1905 = EDGE_LOOP ( 'NONE', ( #4834, #2718, #1984, #3668 ) ) ;
#1906 = CARTESIAN_POINT ( 'NONE',  ( -60.99999999999998579, 14.77083333333333570, 0.9226497308103762673 ) ) ;
#1907 = CARTESIAN_POINT ( 'NONE',  ( -61.13531646874997705, 10.11979166632526805, 1.999225269531026417 ) ) ;
#1908=STYLED_ITEM('',(#11006),#8465);
#1909 = DIRECTION ( 'NONE',  ( 1.000000000000000000, 0.000000000000000000, 0.000000000000000000 ) ) ;
#1910 = CARTESIAN_POINT ( 'NONE',  ( -61.56765823437498142, 15.36979166632526805, 0.7511620957034663704 ) ) ;
#1911 = CARTESIAN_POINT ( 'NONE',  ( -62.99999999999998579, 12.61458333265053611, 2.077350269189627952 ) ) ;
#1912 = CARTESIAN_POINT ( 'NONE',  ( 0.000000000000000000, 0.000000000000000000, 0.000000000000000000 ) ) ;
#1913 = ORIENTED_EDGE ( 'NONE', *, *, #7217, .T. ) ;
#1914 = DIRECTION ( 'NONE',  ( 0.000000000000000000, 0.000000000000000000, 1.000000000000000000 ) ) ;
#1915 = CARTESIAN_POINT ( 'NONE',  ( -61.13531646874997705, 11.80729166632526805, 1.999225269531026417 ) ) ;
#1916 = DIRECTION ( 'NONE',  ( 1.000000000000000000, 0.000000000000000000, 0.000000000000000000 ) ) ;
#1917 = DIRECTION ( 'NONE',  ( 0.000000000000000000, -1.084202172485504434E-16, 1.000000000000000000 ) ) ;
#1918 = ORIENTED_EDGE ( 'NONE', *, *, #2411, .F. ) ;
#1919 = CARTESIAN_POINT ( 'NONE',  ( -61.49999999999998579, 11.20833333333333393, 2.366025403784441927 ) ) ;
#1920 = DIRECTION ( 'NONE',  ( -0.000000000000000000, -1.000000000000000000, -0.000000000000000000 ) ) ;
#1921 = CARTESIAN_POINT ( 'NONE',  ( -61.99999999999998579, 13.82812499965860198, 2.498450539062049724 ) ) ;
#1922 = CARTESIAN_POINT ( 'NONE',  ( -61.49999999999998579, 10.29166666666666785, 0.6339745962155628467 ) ) ;
#1923 = VECTOR ( 'NONE', #9384, 1000.000000000000000 ) ;
#1924 = CARTESIAN_POINT ( 'NONE',  ( -61.49999999999998579, 9.427083332650536107, 2.366025403784441927 ) ) ;
#1925 = VERTEX_POINT ( 'NONE', #1178 ) ;
#1926 = CARTESIAN_POINT ( 'NONE',  ( -60.99999999999998579, 14.02083333333333215, 0.9226497308103762673 ) ) ;
#1927 = AXIS2_PLACEMENT_3D ( 'NONE', #10763, #3154, #2167 ) ;
#1928 = EDGE_CURVE ( 'NONE', #2837, #506, #3848, .T. ) ;
#1929 = EDGE_CURVE ( 'NONE', #10524, #8381, #2909, .T. ) ;
#1930 = CARTESIAN_POINT ( 'NONE',  ( -61.99999999999998579, 10.64062499965860376, 0.5015494609379544944 ) ) ;
#1931 = AXIS2_PLACEMENT_3D ( 'NONE', #7, #8563, #10163 ) ;
#1932 = ORIENTED_EDGE ( 'NONE', *, *, #7786, .F. ) ;
#1933 = CARTESIAN_POINT ( 'NONE',  ( -62.86468353124998032, 10.24479166632526983, 1.000774730468978246 ) ) ;
#1934 = DIRECTION ( 'NONE',  ( 0.000000000000000000, 0.000000000000000000, -1.000000000000000000 ) ) ;
#1935 = APPLICATION_CONTEXT ( 'automotive_design' ) ;
#1936 = AXIS2_PLACEMENT_3D ( 'NONE', #9363, #8538, #6708 ) ;
#1937 = CARTESIAN_POINT ( 'NONE',  ( -61.13531646874998415, 14.14062499965860198, 1.500000000000002220 ) ) ;
#1938 = CARTESIAN_POINT ( 'NONE',  ( -77.99999999999998579, -11.50000000000000711, 8.000000000000000000 ) ) ;
#1939 = EDGE_LOOP ( 'NONE', ( #6034, #3156, #1522, #2323 ) ) ;
#1940 = CARTESIAN_POINT ( 'NONE',  ( -149.9999999999999716, -12.99999999999998757, 0.000000000000000000 ) ) ;
#1941 =( BOUNDED_CURVE ( )  B_SPLINE_CURVE ( 2, ( #1628, #7521, #7415, #6741, #1524 ),
 .UNSPECIFIED., .F., .T. ) 
 B_SPLINE_CURVE_WITH_KNOTS ( ( 3, 2, 3 ),
 ( 0.000000000000000000, 0.005208333333333333044, 0.007812499999999973112 ),
 .UNSPECIFIED. ) 
 CURVE ( )  GEOMETRIC_REPRESENTATION_ITEM ( )  RATIONAL_B_SPLINE_CURVE ( ( 1.000000000000000000, 0.8660254037844387076, 1.000000000000000000, 0.9330127018922200755, 0.9330127018922194093 ) ) 
 REPRESENTATION_ITEM ( '' )  );
#1942 = ORIENTED_EDGE ( 'NONE', *, *, #10570, .F. ) ;
#1943 = LINE ( 'NONE', #3717, #5718 ) ;
#1944 = CARTESIAN_POINT ( 'NONE',  ( -61.56765823437498142, 15.86979166632526628, 0.7511620957034663704 ) ) ;
#1945 = LINE ( 'NONE', #7670, #6987 ) ;
#1946 = CARTESIAN_POINT ( 'NONE',  ( 0.000000000000000000, 0.000000000000000000, -1.886264737416298409 ) ) ;
#1947 = CARTESIAN_POINT ( 'NONE',  ( -49.99999999999998579, -14.00000000000001243, -0.1418111474832540464 ) ) ;
#1948 = ADVANCED_FACE ( 'NONE', ( #5445 ), #8851, .T. ) ;
#1949 = CARTESIAN_POINT ( 'NONE',  ( -61.13531646874997705, 14.16145833299193413, 1.000774730468978468 ) ) ;
#1950 = CARTESIAN_POINT ( 'NONE',  ( -62.86468353124998742, 8.223958332991934128, 1.999225269531025972 ) ) ;
#1951 =( GEOMETRIC_REPRESENTATION_CONTEXT ( 3 ) GLOBAL_UNCERTAINTY_ASSIGNED_CONTEXT ( ( #5811 ) ) GLOBAL_UNIT_ASSIGNED_CONTEXT ( ( #4733, #3743, #6478 ) ) REPRESENTATION_CONTEXT ( 'NONE', 'WORKASPACE' ) );
#1952 = CARTESIAN_POINT ( 'NONE',  ( 145.0000000000000284, -5.500000000000000000, 0.000000000000000000 ) ) ;
#1953 = CARTESIAN_POINT ( 'NONE',  ( -5.895349312889930360E-16, 0.2499999999999998890, 1.454823465665887605 ) ) ;
#1954 = CARTESIAN_POINT ( 'NONE',  ( -61.13531646874998415, 10.64062499965860198, 1.500000000000002220 ) ) ;
#1955 = EDGE_CURVE ( 'NONE', #9681, #1845, #7340, .T. ) ;
#1956 = CARTESIAN_POINT ( 'NONE',  ( -61.06765823437498852, 8.039062499829300990, 1.500000000000002220 ) ) ;
#1957 = EDGE_LOOP ( 'NONE', ( #596, #5706, #4141, #6991 ) ) ;
#1958 = CARTESIAN_POINT ( 'NONE',  ( -60.99999999999998579, 11.19791666598387003, 2.077350269189628840 ) ) ;
#1959 = AXIS2_PLACEMENT_3D ( 'NONE', #975, #1818, #4248 ) ;
#1960 = CARTESIAN_POINT ( 'NONE',  ( -61.49999999999998579, 10.04166666666666785, 0.6339745962155628467 ) ) ;
#1961 = CARTESIAN_POINT ( 'NONE',  ( -62.86468353124999453, 12.20312499965860198, 1.500000000000002220 ) ) ;
#1962 = CARTESIAN_POINT ( 'NONE',  ( -62.86468353124999453, 8.453124999658601979, 1.500000000000002220 ) ) ;
#1963 = LINE ( 'NONE', #6962, #7655 ) ;
#1964 = ORIENTED_EDGE ( 'NONE', *, *, #9119, .F. ) ;
#1965 = CARTESIAN_POINT ( 'NONE',  ( 150.0000000000000000, 8.000000000000000000, 3.000000000000000000 ) ) ;
#1966 = CARTESIAN_POINT ( 'NONE',  ( -61.13531646874998415, 9.890624999658601979, 1.500000000000002220 ) ) ;
#1967 =( LENGTH_UNIT ( ) NAMED_UNIT ( * ) SI_UNIT ( .MILLI., .METRE. ) );
#1968 = CARTESIAN_POINT ( 'NONE',  ( -61.13531646874998415, 14.80729166632526805, 1.999225269531026417 ) ) ;
#1969 = CARTESIAN_POINT ( 'NONE',  ( -61.99999999999998579, 14.65624999931720218, 2.654700538379254571 ) ) ;
#1970 = LINE ( 'NONE', #9577, #10874 ) ;
#1971 = ORIENTED_EDGE ( 'NONE', *, *, #7541, .F. ) ;
#1972 = CARTESIAN_POINT ( 'NONE',  ( 0.5000000000000000000, 0.000000000000000000, 1.928074011315806136 ) ) ;
#1973 = ADVANCED_FACE ( 'NONE', ( #9068 ), #4833, .T. ) ;
#1974 = CARTESIAN_POINT ( 'NONE',  ( -62.86468353124999453, 13.22395833299193235, 1.999225269531025750 ) ) ;
#1975 = CARTESIAN_POINT ( 'NONE',  ( -62.86468353124999453, 8.453124999658601979, 1.500000000000002220 ) ) ;
#1976 = CARTESIAN_POINT ( 'NONE',  ( -62.26794919243111082, 8.323664549684629321, 0.5000000000000025535 ) ) ;
#1977 = EDGE_LOOP ( 'NONE', ( #10642, #6739 ) ) ;
#1978 = CARTESIAN_POINT ( 'NONE',  ( -61.49999999999998579, 11.95833333333333215, 2.366025403784441927 ) ) ;
#1979 = CARTESIAN_POINT ( 'NONE',  ( 190.0000000000000000, -6.123233995736783046E-16, 4.000000000000000000 ) ) ;
#1980 = CARTESIAN_POINT ( 'NONE',  ( -62.43234176562498305, 13.97395833299193413, 0.7511620957034662593 ) ) ;
#1981 = FILL_AREA_STYLE_COLOUR ( '', #9214 ) ;
#1982 = CARTESIAN_POINT ( 'NONE',  ( -62.99999999999998579, 13.87500000000000000, 1.500000000000001998 ) ) ;
#1983 = CARTESIAN_POINT ( 'NONE',  ( -62.49999999999998579, 10.05208333265053611, 0.6339745962155627357 ) ) ;
#1984 = ORIENTED_EDGE ( 'NONE', *, *, #6612, .F. ) ;
#1985 = CARTESIAN_POINT ( 'NONE',  ( -61.49999999999998579, 13.45833333333333215, 2.366025403784441927 ) ) ;
#1986 = CARTESIAN_POINT ( 'NONE',  ( -61.99999999999998579, 9.906249999317202182, 2.500000000000002665 ) ) ;
#1987 = EDGE_CURVE ( 'NONE', #6146, #3291, #10736, .T. ) ;
#1988 = CARTESIAN_POINT ( 'NONE',  ( -62.43234176562499016, 11.49479166632526805, 2.248837904296538071 ) ) ;
#1989 = ORIENTED_EDGE ( 'NONE', *, *, #6880, .T. ) ;
#1990 = AXIS2_PLACEMENT_3D ( 'NONE', #9562, #3499, #838 ) ;
#1991 = CARTESIAN_POINT ( 'NONE',  ( -61.99999999999998579, 9.828124999658600203, 2.498450539062049724 ) ) ;
#1992 = DIRECTION ( 'NONE',  ( -0.000000000000000000, 0.000000000000000000, -1.000000000000000000 ) ) ;
#1993 = EDGE_CURVE ( 'NONE', #10287, #2286, #7346, .T. ) ;
#1994 = CARTESIAN_POINT ( 'NONE',  ( -62.43234176562498305, 13.97395833299193413, 0.7511620957034662593 ) ) ;
#1995 = DIRECTION ( 'NONE',  ( 0.000000000000000000, -0.000000000000000000, 1.000000000000000000 ) ) ;
#1996 = VERTEX_POINT ( 'NONE', #9898 ) ;
#1997 = CIRCLE ( 'NONE', #3066, 1.099999999999989875 ) ;
#1998 = CARTESIAN_POINT ( 'NONE',  ( -105.0000000000000000, 2.500000000000000000, 2.000000000000000000 ) ) ;
#1999 = AXIS2_PLACEMENT_3D ( 'NONE', #9122, #4884, #8287 ) ;
#2000 = ORIENTED_EDGE ( 'NONE', *, *, #3278, .T. ) ;
#2001 = CARTESIAN_POINT ( 'NONE',  ( -62.99999999999998579, 15.11458333265053433, 2.077350269189627952 ) ) ;
#2002 = CARTESIAN_POINT ( 'NONE',  ( -62.49999999999998579, 8.833333333333333925, 0.6339745962155627357 ) ) ;
#2003 = CARTESIAN_POINT ( 'NONE',  ( -61.99999999999998579, 10.18750000000000000, 2.500000000000002665 ) ) ;
#2004 = CARTESIAN_POINT ( 'NONE',  ( -105.0000000000000000, -2.500000000000000000, 4.000000000000000000 ) ) ;
#2005 = CARTESIAN_POINT ( 'NONE',  ( 145.0000000000000284, -5.500000000000000000, 3.000000000000000000 ) ) ;
#2006 = VECTOR ( 'NONE', #117, 1000.000000000000000 ) ;
#2007 = CARTESIAN_POINT ( 'NONE',  ( -61.99999999999999289, 14.45312499965860020, 0.5015494609379544944 ) ) ;
#2008 = VECTOR ( 'NONE', #1065, 1000.000000000000000 ) ;
#2009 = CARTESIAN_POINT ( 'NONE',  ( -62.43234176562498305, 9.911458332991934128, 0.7511620957034662593 ) ) ;
#2010 = CARTESIAN_POINT ( 'NONE',  ( -61.99999999999998579, 11.40624999931720218, 2.500000000000002665 ) ) ;
#2011 = LINE ( 'NONE', #3612, #5286 ) ;
#2012 = CARTESIAN_POINT ( 'NONE',  ( -61.13531646874998415, 10.91145833299193590, 1.000774730468978468 ) ) ;
#2013 = CARTESIAN_POINT ( 'NONE',  ( -62.99999999999998579, 12.12500000000000000, 1.500000000000001998 ) ) ;
#2014 = ORIENTED_EDGE ( 'NONE', *, *, #2239, .F. ) ;
#2015 = DIRECTION ( 'NONE',  ( -0.000000000000000000, -0.000000000000000000, -1.000000000000000000 ) ) ;
#2016 = CARTESIAN_POINT ( 'NONE',  ( -61.73205080756886076, 15.19866454968462932, 2.500000000000003109 ) ) ;
#2017 = AXIS2_PLACEMENT_3D ( 'NONE', #3794, #7184, #10618 ) ;
#2018 = VERTEX_POINT ( 'NONE', #7805 ) ;
#2019 = CARTESIAN_POINT ( 'NONE',  ( -61.49999999999998579, 9.958333333333332149, 2.366025403784441927 ) ) ;
#2020 = CARTESIAN_POINT ( 'NONE',  ( -61.13531646874998415, 13.09895833299193413, 1.000774730468978468 ) ) ;
#2021 = EDGE_CURVE ( 'NONE', #8537, #9717, #5962, .T. ) ;
#2022 = CARTESIAN_POINT ( 'NONE',  ( -61.99999999999999289, 9.390624999658600203, 0.5015494609379544944 ) ) ;
#2023 = CARTESIAN_POINT ( 'NONE',  ( -62.49999999999998579, 8.666666666666666075, 2.366025403784441483 ) ) ;
#2024 = ORIENTED_EDGE ( 'NONE', *, *, #4812, .F. ) ;
#2025 = CARTESIAN_POINT ( 'NONE',  ( -61.49999999999998579, 8.427083332650536107, 2.366025403784441927 ) ) ;
#2026 = CARTESIAN_POINT ( 'NONE',  ( -61.13531646874998415, 10.39062499965860198, 1.500000000000002220 ) ) ;
#2027 = CARTESIAN_POINT ( 'NONE',  ( -62.86468353124999453, 15.95312499965860198, 1.500000000000002220 ) ) ;
#2028 = AXIS2_PLACEMENT_3D ( 'NONE', #10381, #937, #2725 ) ;
#2029 = CARTESIAN_POINT ( 'NONE',  ( -62.99999999999998579, 14.34374999931720041, 1.500000000000001998 ) ) ;
#2030 = CARTESIAN_POINT ( 'NONE',  ( -25.39999999999996305, 0.000000000000000000, 0.000000000000000000 ) ) ;
#2031 = EDGE_LOOP ( 'NONE', ( #10627, #10777, #9434, #3454 ) ) ;
#2032 = ORIENTED_EDGE ( 'NONE', *, *, #5591, .F. ) ;
#2033 = CARTESIAN_POINT ( 'NONE',  ( -62.43234176562499016, 13.24479166632526805, 2.248837904296538071 ) ) ;
#2034 = CARTESIAN_POINT ( 'NONE',  ( -61.13531646874998415, 8.307291666325269830, 1.999225269531026417 ) ) ;
#2035 = DIRECTION ( 'NONE',  ( -0.000000000000000000, -1.000000000000000000, -0.000000000000000000 ) ) ;
#2036 = ORIENTED_EDGE ( 'NONE', *, *, #4732, .T. ) ;
#2037 = CARTESIAN_POINT ( 'NONE',  ( -60.99999999999998579, 12.02083333333333393, 0.9226497308103762673 ) ) ;
#2038 = CARTESIAN_POINT ( 'NONE',  ( -99.99999999999998579, 15.67949192431120053, -2.000000000000000000 ) ) ;
#2039 = CARTESIAN_POINT ( 'NONE',  ( -62.43234176562498305, 14.22395833299193413, 0.7511620957034662593 ) ) ;
#2040 =( LENGTH_UNIT ( ) NAMED_UNIT ( * ) SI_UNIT ( .MILLI., .METRE. ) );
#2041 = CARTESIAN_POINT ( 'NONE',  ( -61.49999999999998579, 10.95833333333333393, 2.366025403784441927 ) ) ;
#2042 = EDGE_CURVE ( 'NONE', #10433, #1452, #1970, .T. ) ;
#2043 = CARTESIAN_POINT ( 'NONE',  ( -61.49999999999998579, 10.51041666598387003, 0.6339745962155628467 ) ) ;
#2044 = ORIENTED_EDGE ( 'NONE', *, *, #9484, .T. ) ;
#2045 = DIRECTION ( 'NONE',  ( -0.000000000000000000, -1.000000000000000000, -0.000000000000000000 ) ) ;
#2046 = DIRECTION ( 'NONE',  ( 1.000000000000000000, 0.000000000000000000, 0.000000000000000000 ) ) ;
#2047 = SHAPE_REPRESENTATION ( 'moving jaw', ( #2307 ), #4948 ) ;
#2048 = CARTESIAN_POINT ( 'NONE',  ( -62.43234176562498305, 12.41145833299193413, 0.7511620957034662593 ) ) ;
#2049 = ORIENTED_EDGE ( 'NONE', *, *, #7739, .T. ) ;
#2050 = CARTESIAN_POINT ( 'NONE',  ( -61.99999999999998579, 9.953124999658601979, 0.5015494609379544944 ) ) ;
#2051 = CARTESIAN_POINT ( 'NONE',  ( 190.0000000000000000, 0.000000000000000000, 2.000000000000000000 ) ) ;
#2052 = CARTESIAN_POINT ( 'NONE',  ( -61.99999999999998579, 13.95312499965860198, 0.5015494609379544944 ) ) ;
#2053 = CARTESIAN_POINT ( 'NONE',  ( -120.0000000000000000, -15.00000000000001421, -2.000000000000000000 ) ) ;
#2054 = EDGE_LOOP ( 'NONE', ( #2057, #2218, #8952, #10553 ) ) ;
#2055 = CARTESIAN_POINT ( 'NONE',  ( 150.0000000000000000, -8.000000000000000000, 6.000000000000000000 ) ) ;
#2056 = EDGE_CURVE ( 'NONE', #3973, #3104, #6857, .T. ) ;
#2057 = ORIENTED_EDGE ( 'NONE', *, *, #5007, .F. ) ;
#2058 = CARTESIAN_POINT ( 'NONE',  ( -60.99999999999998579, 8.729166666666666075, 2.077350269189628840 ) ) ;
#2059 = CARTESIAN_POINT ( 'NONE',  ( -62.99999999999998579, 8.145833333333332149, 2.077350269189627952 ) ) ;
#2060 = LINE ( 'NONE', #9889, #6469 ) ;
#2061 = DIRECTION ( 'NONE',  ( 0.000000000000000000, 1.000000000000000000, 0.000000000000000000 ) ) ;
#2062 = CARTESIAN_POINT ( 'NONE',  ( -139.9999999999999716, -43.00000000000000000, 3.000000000000000000 ) ) ;
#2063 = CARTESIAN_POINT ( 'NONE',  ( -61.13531646874997705, 14.91145833299193768, 1.000774730468978468 ) ) ;
#2064 = CARTESIAN_POINT ( 'NONE',  ( -61.99999999999998579, 9.640624999658600203, 0.5015494609379544944 ) ) ;
#2065 = PRODUCT_DEFINITION_CONTEXT ( 'detailed design', #3715, 'design' ) ;
#2066 = CARTESIAN_POINT ( 'NONE',  ( -61.49999999999998579, 12.01041666598387003, 0.6339745962155628467 ) ) ;
#2067 = DIRECTION ( 'NONE',  ( 0.000000000000000000, -1.000000000000000000, 0.000000000000000000 ) ) ;
#2068 = CARTESIAN_POINT ( 'NONE',  ( -61.13531646874998415, 10.86979166632526805, 1.999225269531026417 ) ) ;
#2069 = CYLINDRICAL_SURFACE ( 'NONE', #8218, 30.00000000000000000 ) ;
#2070 = VERTEX_POINT ( 'NONE', #9406 ) ;
#2071 = CARTESIAN_POINT ( 'NONE',  ( -62.49999999999998579, 14.41666666666666785, 2.366025403784441483 ) ) ;
#2072 = DIRECTION ( 'NONE',  ( 1.000000000000000000, -0.000000000000000000, 0.000000000000000000 ) ) ;
#2073 = EDGE_CURVE ( 'NONE', #427, #7723, #5227, .T. ) ;
#2074 = ORIENTED_EDGE ( 'NONE', *, *, #388, .F. ) ;
#2075 = CARTESIAN_POINT ( 'NONE',  ( -61.99999999999998579, 9.937500000000000000, 2.500000000000002665 ) ) ;
#2076 = CARTESIAN_POINT ( 'NONE',  ( -61.13531646874998415, 12.57812499965860198, 1.500000000000002220 ) ) ;
#2077 = CARTESIAN_POINT ( 'NONE',  ( -62.43234176562498305, 10.66145833299193413, 0.7511620957034662593 ) ) ;
#2078 = ORIENTED_EDGE ( 'NONE', *, *, #7061, .F. ) ;
#2079 = DIRECTION ( 'NONE',  ( -0.000000000000000000, 1.000000000000000000, -0.000000000000000000 ) ) ;
#2080 = CARTESIAN_POINT ( 'NONE',  ( -61.56765823437498142, 10.68229166632526805, 0.7511620957034663704 ) ) ;
#2081 = APPLICATION_PROTOCOL_DEFINITION ( 'draft international standard', 'automotive_design', 1998, #6771 ) ;
#2082 = CARTESIAN_POINT ( 'NONE',  ( -61.56765823437498142, 15.86979166632526628, 0.7511620957034663704 ) ) ;
#2083 = CARTESIAN_POINT ( 'NONE',  ( -61.99999999999998579, 14.53124999931720041, 0.3452994616207497591 ) ) ;
#2084 = DIRECTION ( 'NONE',  ( -0.000000000000000000, -0.000000000000000000, 1.000000000000000000 ) ) ;
#2085 = ORIENTED_EDGE ( 'NONE', *, *, #4471, .T. ) ;
#2086 = DIRECTION ( 'NONE',  ( -1.000000000000000000, 0.000000000000000000, -0.000000000000000000 ) ) ;
#2087 = ORIENTED_EDGE ( 'NONE', *, *, #4800, .F. ) ;
#2088 = EDGE_CURVE ( 'NONE', #5975, #8381, #10227, .T. ) ;
#2089 = CARTESIAN_POINT ( 'NONE',  ( -62.86468353124999453, 13.20312499965860198, 1.500000000000002220 ) ) ;
#2090 = CARTESIAN_POINT ( 'NONE',  ( -49.99999999999998579, -14.00000000000001243, 3.141811147483255073 ) ) ;
#2091 = DIRECTION ( 'NONE',  ( -0.000000000000000000, -0.000000000000000000, -1.000000000000000000 ) ) ;
#2092 = ORIENTED_EDGE ( 'NONE', *, *, #9950, .F. ) ;
#2093 = CARTESIAN_POINT ( 'NONE',  ( -60.99999999999998579, 12.75000000000000178, 1.500000000000002220 ) ) ;
#2094 = DIRECTION ( 'NONE',  ( 0.000000000000000000, -0.000000000000000000, 1.000000000000000000 ) ) ;
#2095 = CARTESIAN_POINT ( 'NONE',  ( -62.43234176562499016, 14.80729166632526805, 2.248837904296538071 ) ) ;
#2096 = EDGE_CURVE ( 'NONE', #5931, #918, #4917, .T. ) ;
#2097 = CARTESIAN_POINT ( 'NONE',  ( -62.49999999999998579, 10.63541666598387003, 2.366025403784441483 ) ) ;
#2098 = ORIENTED_EDGE ( 'NONE', *, *, #4861, .F. ) ;
#2099 =( GEOMETRIC_REPRESENTATION_CONTEXT ( 3 ) GLOBAL_UNCERTAINTY_ASSIGNED_CONTEXT ( ( #7955 ) ) GLOBAL_UNIT_ASSIGNED_CONTEXT ( ( #3880, #2217, #6383 ) ) REPRESENTATION_CONTEXT ( 'NONE', 'WORKASPACE' ) );
#2100 = EDGE_CURVE ( 'NONE', #4938, #3792, #6020, .T. ) ;
#2101 = CARTESIAN_POINT ( 'NONE',  ( 0.000000000000000000, 0.000000000000000000, 3.000000000000000000 ) ) ;
#2102 = CARTESIAN_POINT ( 'NONE',  ( -62.86468353124998032, 12.68229166632526983, 1.000774730468978246 ) ) ;
#2103 = EDGE_CURVE ( 'NONE', #9392, #1175, #604, .T. ) ;
#2104 = ORIENTED_EDGE ( 'NONE', *, *, #9938, .F. ) ;
#2105 = CARTESIAN_POINT ( 'NONE',  ( -61.13531646874998415, 10.86979166632526805, 1.999225269531026417 ) ) ;
#2106 = CARTESIAN_POINT ( 'NONE',  ( -62.26794919243111082, 15.64508544963257108, 2.500000000000003109 ) ) ;
#2107 = AXIS2_PLACEMENT_3D ( 'NONE', #5307, #266, #3649 ) ;
#2108 = CARTESIAN_POINT ( 'NONE',  ( -62.43234176562499016, 14.30729166632526983, 2.248837904296538071 ) ) ;
#2109 = CARTESIAN_POINT ( 'NONE',  ( -144.9999999999999147, -16.54248688935410883, 0.000000000000000000 ) ) ;
#2110 = ORIENTED_EDGE ( 'NONE', *, *, #2887, .F. ) ;
#2111 =( BOUNDED_CURVE ( )  B_SPLINE_CURVE ( 2, ( #4831, #5774, #10049, #4051, #9169, #4722, #8337, #4106, #9897 ),
 .UNSPECIFIED., .F., .T. ) 
 B_SPLINE_CURVE_WITH_KNOTS ( ( 3, 2, 2, 2, 3 ),
 ( 0.9140625000000000000, 0.9166666666666666297, 0.9218750000000000000, 0.9270833333333333703, 0.9296875000000000000 ),
 .UNSPECIFIED. ) 
 CURVE ( )  GEOMETRIC_REPRESENTATION_ITEM ( )  RATIONAL_B_SPLINE_CURVE ( ( 0.9330127018922194093, 0.9330127018922194093, 1.000000000000000000, 0.8660254037844387076, 1.000000000000000000, 0.8660254037844387076, 1.000000000000000000, 0.9330127018922194093, 0.9330127018922194093 ) ) 
 REPRESENTATION_ITEM ( '' )  );
#2112 = CARTESIAN_POINT ( 'NONE',  ( -61.49999999999998579, 10.54166666666666607, 0.6339745962155628467 ) ) ;
#2113 = AXIS2_PLACEMENT_3D ( 'NONE', #1593, #5867, #8534 ) ;
#2114 = ORIENTED_EDGE ( 'NONE', *, *, #2619, .T. ) ;
#2115 = DIRECTION ( 'NONE',  ( 0.000000000000000000, -1.000000000000000000, 0.000000000000000000 ) ) ;
#2116 = CARTESIAN_POINT ( 'NONE',  ( -61.49999999999998579, 8.958333333333333925, 2.366025403784441927 ) ) ;
#2117 = CARTESIAN_POINT ( 'NONE',  ( -61.99999999999997868, 9.656249999317202182, 2.500000000000002665 ) ) ;
#2118 = DIRECTION ( 'NONE',  ( -0.000000000000000000, -0.000000000000000000, 1.000000000000000000 ) ) ;
#2119 = CARTESIAN_POINT ( 'NONE',  ( -62.26794919243111082, 8.926335450315370679, 2.500000000000004885 ) ) ;
#2120 = VECTOR ( 'NONE', #1415, 1000.000000000000000 ) ;
#2121 = CARTESIAN_POINT ( 'NONE',  ( -62.86468353124999453, 9.703124999658601979, 1.500000000000002220 ) ) ;
#2122 =( LENGTH_UNIT ( ) NAMED_UNIT ( * ) SI_UNIT ( .MILLI., .METRE. ) );
#2123 = DIRECTION ( 'NONE',  ( 1.000000000000000000, 0.000000000000000000, 0.000000000000000000 ) ) ;
#2124 = CARTESIAN_POINT ( 'NONE',  ( -62.86468353124999453, 10.51562499965860198, 1.500000000000002220 ) ) ;
#2125 =( GEOMETRIC_REPRESENTATION_CONTEXT ( 3 ) GLOBAL_UNCERTAINTY_ASSIGNED_CONTEXT ( ( #5383 ) ) GLOBAL_UNIT_ASSIGNED_CONTEXT ( ( #7766, #2711, #6151 ) ) REPRESENTATION_CONTEXT ( 'NONE', 'WORKASPACE' ) );
#2126 = FACE_OUTER_BOUND ( 'NONE', #7599, .T. ) ;
#2127 = EDGE_LOOP ( 'NONE', ( #10724, #4904, #5313, #1006 ) ) ;
#2128 = ADVANCED_FACE ( 'NONE', ( #1745 ), #2802, .T. ) ;
#2129 = CARTESIAN_POINT ( 'NONE',  ( 146.0999999999999943, 5.500000000000000000, 6.000000000000000000 ) ) ;
#2130 = DIRECTION ( 'NONE',  ( -0.000000000000000000, -0.000000000000000000, 1.000000000000000000 ) ) ;
#2131 = AXIS2_PLACEMENT_3D ( 'NONE', #7736, #5056, #2617 ) ;
#2132 = ADVANCED_FACE ( 'NONE', ( #3460 ), #6275, .T. ) ;
#2133 = ORIENTED_EDGE ( 'NONE', *, *, #1855, .T. ) ;
#2134 = CARTESIAN_POINT ( 'NONE',  ( -62.99999999999998579, 10.11458333265053611, 2.077350269189627952 ) ) ;
#2135 = CARTESIAN_POINT ( 'NONE',  ( -61.13531646874998415, 12.59895833299193590, 1.000774730468978468 ) ) ;
#2136 = CARTESIAN_POINT ( 'NONE',  ( -61.56765823437498852, 10.78645833299193413, 2.248837904296538515 ) ) ;
#2137 = AXIS2_PLACEMENT_3D ( 'NONE', #3458, #2631, #6017 ) ;
#2138 = CARTESIAN_POINT ( 'NONE',  ( -61.13531646874998415, 8.109374999658601979, 1.500000000000002220 ) ) ;
#2139 = ORIENTED_EDGE ( 'NONE', *, *, #8375, .F. ) ;
#2140 = CARTESIAN_POINT ( 'NONE',  ( -61.99999999999998579, 14.99999999999998579, 1.500000000000002220 ) ) ;
#2141 = CARTESIAN_POINT ( 'NONE',  ( -62.86468353124999453, 11.76562499965860198, 1.500000000000002220 ) ) ;
#2142 = CARTESIAN_POINT ( 'NONE',  ( -62.86468353124999453, 15.20312499965860020, 1.500000000000002220 ) ) ;
#2143 = EDGE_CURVE ( 'NONE', #9954, #8835, #1486, .T. ) ;
#2144 = AXIS2_PLACEMENT_3D ( 'NONE', #4502, #10617, #3015 ) ;
#2145 = CARTESIAN_POINT ( 'NONE',  ( -60.99999999999998579, 14.73958333265053433, 0.9226497308103762673 ) ) ;
#2146 = CARTESIAN_POINT ( 'NONE',  ( -60.99999999999998579, 14.73958333265053433, 0.9226497308103762673 ) ) ;
#2147 = ORIENTED_EDGE ( 'NONE', *, *, #4001, .T. ) ;
#2148 = CARTESIAN_POINT ( 'NONE',  ( -32.99999999999998579, -14.00000000000000888, -2.000000000000000000 ) ) ;
#2149 = ORIENTED_EDGE ( 'NONE', *, *, #4021, .T. ) ;
#2150 = PRODUCT_DEFINITION_FORMATION_WITH_SPECIFIED_SOURCE ( 'ANY', '', #7593, .NOT_KNOWN. ) ;
#2151 = CARTESIAN_POINT ( 'NONE',  ( -61.99999999999999289, 12.76562499965860198, 2.498450539062049724 ) ) ;
#2152 = CARTESIAN_POINT ( 'NONE',  ( -61.56765823437498142, 8.369791666325268054, 0.7511620957034663704 ) ) ;
#2153 = CARTESIAN_POINT ( 'NONE',  ( -62.49999999999998579, 10.55208333265053611, 0.6339745962155627357 ) ) ;
#2154 = EDGE_LOOP ( 'NONE', ( #269, #8721, #5421, #5391 ) ) ;
#2155 = CARTESIAN_POINT ( 'NONE',  ( -61.49999999999998579, 12.20833333333333393, 2.366025403784441927 ) ) ;
#2156 = CARTESIAN_POINT ( 'NONE',  ( -61.73205080756886076, 9.051335450315368902, 0.5000000000000014433 ) ) ;
#2157 = CARTESIAN_POINT ( 'NONE',  ( -134.9999999999999147, 8.000000000000000000, 3.000000000000000000 ) ) ;
#2158 = CARTESIAN_POINT ( 'NONE',  ( -62.99999999999998579, 10.57291666598387181, 0.9226497308103756012 ) ) ;
#2159 = ORIENTED_EDGE ( 'NONE', *, *, #1003, .F. ) ;
#2160 = CARTESIAN_POINT ( 'NONE',  ( -61.99999999999998579, 14.81250000000000000, 0.5000000000000013323 ) ) ;
#2161 = CARTESIAN_POINT ( 'NONE',  ( -62.43234176562499016, 13.24479166632526805, 2.248837904296538071 ) ) ;
#2162 = EDGE_CURVE ( 'NONE', #9310, #7235, #244, .T. ) ;
#2163 = CARTESIAN_POINT ( 'NONE',  ( -61.73205080756886076, 15.94866454968462932, 2.500000000000003109 ) ) ;
#2164 = VERTEX_POINT ( 'NONE', #1858 ) ;
#2165 = EDGE_CURVE ( 'NONE', #8943, #4570, #7621, .T. ) ;
#2166 = CARTESIAN_POINT ( 'NONE',  ( -61.56765823437498142, 9.682291666325268054, 0.7511620957034663704 ) ) ;
#2167 = DIRECTION ( 'NONE',  ( 0.000000000000000000, -0.000000000000000000, -1.000000000000000000 ) ) ;
#2168 = CARTESIAN_POINT ( 'NONE',  ( -61.56765823437498852, 15.84895833299193590, 2.248837904296538515 ) ) ;
#2169 = CYLINDRICAL_SURFACE ( 'NONE', #5717, 0.9999999999999981126 ) ;
#2170 = ORIENTED_EDGE ( 'NONE', *, *, #9568, .T. ) ;
#2171 = ORIENTED_EDGE ( 'NONE', *, *, #6545, .T. ) ;
#2172 = DIRECTION ( 'NONE',  ( 0.000000000000000000, 0.000000000000000000, -1.000000000000000000 ) ) ;
#2173 = CARTESIAN_POINT ( 'NONE',  ( -61.49999999999998579, 9.208333333333333925, 2.366025403784441927 ) ) ;
#2174 = CARTESIAN_POINT ( 'NONE',  ( 3.489067535589073648E-18, 0.000000000000000000, 0.000000000000000000 ) ) ;
#2175 = DIRECTION ( 'NONE',  ( 0.000000000000000000, 0.000000000000000000, -1.000000000000000000 ) ) ;
#2176 = LINE ( 'NONE', #567, #4928 ) ;
#2177 = CARTESIAN_POINT ( 'NONE',  ( -61.13531646874998415, 9.807291666325268054, 1.999225269531026417 ) ) ;
#2178 =( BOUNDED_CURVE ( )  B_SPLINE_CURVE ( 2, ( #10729, #4877, #5769, #6460, #6567, #8279, #1548, #2230, #10773 ),
 .UNSPECIFIED., .F., .F. ) 
 B_SPLINE_CURVE_WITH_KNOTS ( ( 3, 2, 2, 2, 3 ),
 ( 0.5234375000000000000, 0.5260416666666666297, 0.5312500000000000000, 0.5364583333333333703, 0.5390625000000000000 ),
 .UNSPECIFIED. ) 
 CURVE ( )  GEOMETRIC_REPRESENTATION_ITEM ( )  RATIONAL_B_SPLINE_CURVE ( ( 0.9330127018922194093, 0.9330127018922194093, 1.000000000000000000, 0.8660254037844387076, 1.000000000000000000, 0.8660254037844387076, 1.000000000000000000, 0.9330127018922194093, 0.9330127018922194093 ) ) 
 REPRESENTATION_ITEM ( '' )  );
#2179 = CARTESIAN_POINT ( 'NONE',  ( -60.99999999999998579, 15.46874999931720218, 1.500000000000002220 ) ) ;
#2180 = VECTOR ( 'NONE', #5441, 1000.000000000000000 ) ;
#2181 = ADVANCED_FACE ( 'NONE', ( #3629 ), #6809, .F. ) ;
#2182 = VECTOR ( 'NONE', #727, 1000.000000000000000 ) ;
#2183 = CARTESIAN_POINT ( 'NONE',  ( -61.56765823437498142, 12.18229166632526628, 0.7511620957034663704 ) ) ;
#2184 = DIRECTION ( 'NONE',  ( 1.000000000000000000, -0.000000000000000000, -0.000000000000000000 ) ) ;
#2185 = EDGE_LOOP ( 'NONE', ( #5410, #8896, #7323, #9641 ) ) ;
#2186 = DIRECTION ( 'NONE',  ( 1.000000000000000000, -1.734723475976805517E-15, 0.000000000000000000 ) ) ;
#2187 = CARTESIAN_POINT ( 'NONE',  ( -61.99999999999998579, 12.68750000000000000, 2.500000000000002665 ) ) ;
#2188 = VERTEX_POINT ( 'NONE', #1417 ) ;
#2189 = AXIS2_PLACEMENT_3D ( 'NONE', #6956, #9339, #10337 ) ;
#2190 = CARTESIAN_POINT ( 'NONE',  ( -61.99999999999998579, 10.28124999931720218, 0.5000000000000013323 ) ) ;
#2191 = CARTESIAN_POINT ( 'NONE',  ( -61.56765823437498852, 13.78645833299193413, 2.248837904296538515 ) ) ;
#2192 = CIRCLE ( 'NONE', #5903, 25.99999999999999645 ) ;
#2193 = CARTESIAN_POINT ( 'NONE',  ( -62.86468353124999453, 9.973958332991932352, 1.999225269531025750 ) ) ;
#2194 = CARTESIAN_POINT ( 'NONE',  ( -62.99999999999998579, 8.625000000000000000, 1.500000000000001998 ) ) ;
#2195 = ORIENTED_EDGE ( 'NONE', *, *, #1204, .F. ) ;
#2196 = DIRECTION ( 'NONE',  ( 0.000000000000000000, 0.000000000000000000, 1.000000000000000000 ) ) ;
#2197 = CARTESIAN_POINT ( 'NONE',  ( -62.86468353124999453, 11.53645833299193413, 1.999225269531025750 ) ) ;
#2198 = APPLICATION_PROTOCOL_DEFINITION ( 'draft international standard', 'automotive_design', 1998, #10086 ) ;
#2199 = FACE_OUTER_BOUND ( 'NONE', #4921, .T. ) ;
#2200 = CARTESIAN_POINT ( 'NONE',  ( -61.49999999999998579, 14.92708333265053611, 2.366025403784441927 ) ) ;
#2201 = CARTESIAN_POINT ( 'NONE',  ( 0.5477065543514035850, 0.000000000000000000, 0.000000000000000000 ) ) ;
#2202 = VERTEX_POINT ( 'NONE', #3083 ) ;
#2203 = CARTESIAN_POINT ( 'NONE',  ( -60.99999999999998579, 15.19791666598387359, 2.077350269189628840 ) ) ;
#2204 = VERTEX_POINT ( 'NONE', #10463 ) ;
#2205 = CARTESIAN_POINT ( 'NONE',  ( -62.86468353124999453, 13.47395833299193413, 1.999225269531025750 ) ) ;
#2206 = CARTESIAN_POINT ( 'NONE',  ( -61.99999999999998579, 8.765624999658601979, 2.498450539062049724 ) ) ;
#2207 = CARTESIAN_POINT ( 'NONE',  ( -61.99999999999998579, 8.000000000000000000, 1.500000000000002220 ) ) ;
#2208 = VERTEX_POINT ( 'NONE', #6251 ) ;
#2209 = CARTESIAN_POINT ( 'NONE',  ( -62.49999999999998579, 12.66666666666666607, 2.366025403784441483 ) ) ;
#2210 = AXIS2_PLACEMENT_3D ( 'NONE', #2953, #6816, #5073 ) ;
#2211 = CARTESIAN_POINT ( 'NONE',  ( -62.26794919243110371, 8.542414549001833279, 0.5000000000000032196 ) ) ;
#2212 = CARTESIAN_POINT ( 'NONE',  ( -60.99999999999998579, 15.02083333333333393, 0.9226497308103762673 ) ) ;
#2213 = CARTESIAN_POINT ( 'NONE',  ( -60.99999999999998579, 10.73958333265053611, 0.9226497308103762673 ) ) ;
#2214 = ORIENTED_EDGE ( 'NONE', *, *, #5371, .F. ) ;
#2215 = CARTESIAN_POINT ( 'NONE',  ( 0.5000000000000000000, 0.000000000000000000, 0.000000000000000000 ) ) ;
#2216 = CARTESIAN_POINT ( 'NONE',  ( -61.56765823437498852, 13.03645833299193413, 2.248837904296538515 ) ) ;
#2217 =( NAMED_UNIT ( * ) PLANE_ANGLE_UNIT ( ) SI_UNIT ( $, .RADIAN. ) );
#2218 = ORIENTED_EDGE ( 'NONE', *, *, #5229, .F. ) ;
#2219 = CARTESIAN_POINT ( 'NONE',  ( -61.13531646874998415, 11.64062499965860198, 1.500000000000002220 ) ) ;
#2220 = DIRECTION ( 'NONE',  ( -0.000000000000000000, -1.000000000000000000, -0.000000000000000000 ) ) ;
#2221 = CARTESIAN_POINT ( 'NONE',  ( -62.86468353124998742, 15.53645833299193590, 1.999225269531025972 ) ) ;
#2222 = VERTEX_POINT ( 'NONE', #7250 ) ;
#2223 = CARTESIAN_POINT ( 'NONE',  ( -61.99999999999998579, 16.00000000000000000, 1.500000000000002220 ) ) ;
#2224 = EDGE_CURVE ( 'NONE', #192, #2429, #7198, .T. ) ;
#2225 = ORIENTED_EDGE ( 'NONE', *, *, #10290, .T. ) ;
#2226 = FACE_OUTER_BOUND ( 'NONE', #4710, .T. ) ;
#2227 = CARTESIAN_POINT ( 'NONE',  ( -62.49999999999998579, 10.33333333333333393, 0.6339745962155627357 ) ) ;
#2228 = CARTESIAN_POINT ( 'NONE',  ( -61.99999999999998579, 9.531249999317202182, 0.5000000000000013323 ) ) ;
#2229 = CARTESIAN_POINT ( 'NONE',  ( -60.99999999999998579, 8.500000000000000000, 1.500000000000002220 ) ) ;
#2230 = CARTESIAN_POINT ( 'NONE',  ( -61.73205080756886076, 12.30133545031537068, 0.5000000000000014433 ) ) ;
#2231 = CARTESIAN_POINT ( 'NONE',  ( 150.0000000000000000, 8.000000000000000000, 3.000000000000000000 ) ) ;
#2232 = CARTESIAN_POINT ( 'NONE',  ( -62.86468353124998032, 11.49479166632526805, 1.000774730468978246 ) ) ;
#2233 = DIRECTION ( 'NONE',  ( -0.000000000000000000, -0.000000000000000000, -1.000000000000000000 ) ) ;
#2234 = VERTEX_POINT ( 'NONE', #4687 ) ;
#2235 = CARTESIAN_POINT ( 'NONE',  ( -61.99999999999998579, 16.00000000000000000, 0.5000000000000041078 ) ) ;
#2236 = CARTESIAN_POINT ( 'NONE',  ( -60.99999999999998579, 15.27083333333333393, 0.9226497308103762673 ) ) ;
#2237 = VERTEX_POINT ( 'NONE', #3808 ) ;
#2238 = CARTESIAN_POINT ( 'NONE',  ( 195.0000000000000000, 0.000000000000000000, 4.000000000000000000 ) ) ;
#2239 = EDGE_CURVE ( 'NONE', #6280, #3475, #9824, .T. ) ;
#2240 = CARTESIAN_POINT ( 'NONE',  ( -61.99999999999998579, 14.14062499965860020, 0.5015494609379544944 ) ) ;
#2241 = CARTESIAN_POINT ( 'NONE',  ( -62.86468353124998032, 10.43229166632526983, 1.000774730468978024 ) ) ;
#2242 = SURFACE_STYLE_FILL_AREA ( #7135 ) ;
#2243 =( BOUNDED_CURVE ( )  B_SPLINE_CURVE ( 2, ( #8638, #4342, #5817, #9216, #2640, #2753, #305, #6977, #10041 ),
 .UNSPECIFIED., .F., .T. ) 
 B_SPLINE_CURVE_WITH_KNOTS ( ( 3, 2, 2, 2, 3 ),
 ( 0.9296875000000000000, 0.9322916666666666297, 0.9375000000000000000, 0.9427083333333333703, 0.9453125000000000000 ),
 .UNSPECIFIED. ) 
 CURVE ( )  GEOMETRIC_REPRESENTATION_ITEM ( )  RATIONAL_B_SPLINE_CURVE ( ( 0.9330127018922194093, 0.9330127018922194093, 1.000000000000000000, 0.8660254037844387076, 1.000000000000000000, 0.8660254037844387076, 1.000000000000000000, 0.9330127018922194093, 0.9330127018922194093 ) ) 
 REPRESENTATION_ITEM ( '' )  );
#2244 = EDGE_LOOP ( 'NONE', ( #7454, #9194, #6845, #916 ) ) ;
#2245 = PLANE ( 'NONE',  #7427 ) ;
#2246 = CARTESIAN_POINT ( 'NONE',  ( -62.43234176562498305, 11.22395833299193590, 0.7511620957034662593 ) ) ;
#2247 = CONTEXT_DEPENDENT_SHAPE_REPRESENTATION ( #8326, #6625 ) ;
#2248 = CARTESIAN_POINT ( 'NONE',  ( -105.0000000000000000, 2.500000000000000000, 4.000000000000000000 ) ) ;
#2249 = CARTESIAN_POINT ( 'NONE',  ( -61.99999999999998579, 15.28124999931720218, 0.3452994616207497591 ) ) ;
#2250 = DIRECTION ( 'NONE',  ( -1.000000000000000000, -0.000000000000000000, -0.000000000000000000 ) ) ;
#2251 = VERTEX_POINT ( 'NONE', #2864 ) ;
#2252 = CARTESIAN_POINT ( 'NONE',  ( 146.0000000000000284, -5.500000000000000000, 3.000000000000000000 ) ) ;
#2253 = CARTESIAN_POINT ( 'NONE',  ( -60.99999999999998579, 15.21874999931720218, 1.500000000000002220 ) ) ;
#2254 = EDGE_LOOP ( 'NONE', ( #1322, #9808, #4811, #8979, #8645, #4632, #1942, #4154, #7191, #4501 ) ) ;
#2255 = CARTESIAN_POINT ( 'NONE',  ( -62.43234176562499016, 14.49479166632526983, 2.248837904296538071 ) ) ;
#2256 = CARTESIAN_POINT ( 'NONE',  ( -61.13531646874998415, 9.848958332991934128, 1.000774730468978468 ) ) ;
#2257 = DIRECTION ( 'NONE',  ( -1.000000000000000000, 0.000000000000000000, 0.000000000000000000 ) ) ;
#2258 = VERTEX_POINT ( 'NONE', #8094 ) ;
#2259 = CARTESIAN_POINT ( 'NONE',  ( -61.99999999999998579, 14.18749999999999822, 2.654700538379254571 ) ) ;
#2260 = DIRECTION ( 'NONE',  ( 0.000000000000000000, 0.000000000000000000, -1.000000000000000000 ) ) ;
#2261 = CARTESIAN_POINT ( 'NONE',  ( -60.99999999999998579, 11.96874999931720218, 1.500000000000002220 ) ) ;
#2262 = ADVANCED_FACE ( 'NONE', ( #7082 ), #360, .T. ) ;
#2263 = DIRECTION ( 'NONE',  ( 1.000000000000000000, -0.000000000000000000, -0.000000000000000000 ) ) ;
#2264 = CARTESIAN_POINT ( 'NONE',  ( -62.86468353124998032, 13.18229166632526805, 1.000774730468978246 ) ) ;
#2265 = CARTESIAN_POINT ( 'NONE',  ( 1.314929834301322591E-16, 0.000000000000000000, 0.000000000000000000 ) ) ;
#2266 = EDGE_CURVE ( 'NONE', #5113, #7871, #5189, .T. ) ;
#2267 = ORIENTED_EDGE ( 'NONE', *, *, #6909, .T. ) ;
#2268 = CARTESIAN_POINT ( 'NONE',  ( -62.43234176562499016, 11.80729166632526805, 2.248837904296538071 ) ) ;
#2269 = LINE ( 'NONE', #7383, #8310 ) ;
#2270 = PRODUCT ( 'slotted pan head screw_iso_ISO 1580 - M2 x 6 - 6N', 'slotted pan head screw_iso_ISO 1580 - M2 x 6 - 6N', '', ( #2861 ) ) ;
#2271 = ADVANCED_FACE ( 'NONE', ( #3746 ), #10579, .T. ) ;
#2272 = CARTESIAN_POINT ( 'NONE',  ( -62.43234176562498305, 15.72395833299193590, 0.7511620957034662593 ) ) ;
#2273 = VERTEX_POINT ( 'NONE', #5629 ) ;
#2274 = CARTESIAN_POINT ( 'NONE',  ( -61.99999999999998579, 11.78124999931720218, 0.5000000000000013323 ) ) ;
#2275 = VECTOR ( 'NONE', #8665, 1000.000000000000000 ) ;
#2276 = ORIENTED_EDGE ( 'NONE', *, *, #9119, .T. ) ;
#2277 = CARTESIAN_POINT ( 'NONE',  ( -61.99999999999998579, 9.906249999317202182, 2.500000000000002665 ) ) ;
#2278 = CARTESIAN_POINT ( 'NONE',  ( -60.99999999999998579, 9.750000000000000000, 1.500000000000002220 ) ) ;
#2279 = DIRECTION ( 'NONE',  ( 0.8571673013836855759, 1.049727191973305270E-16, -0.5150380737757257466 ) ) ;
#2280 = CARTESIAN_POINT ( 'NONE',  ( -61.73205080756886076, 14.91741454900183150, 2.500000000000003109 ) ) ;
#2281 = CARTESIAN_POINT ( 'NONE',  ( -62.99999999999998579, 14.84374999931720218, 1.500000000000001998 ) ) ;
#2282 = CARTESIAN_POINT ( 'NONE',  ( -62.99999999999998579, 15.84374999931720218, 1.500000000000001998 ) ) ;
#2283 = AXIS2_PLACEMENT_3D ( 'NONE', #8664, #6785, #2501 ) ;
#2284 = CARTESIAN_POINT ( 'NONE',  ( -62.86468353124999453, 11.76562499965860198, 1.500000000000002220 ) ) ;
#2285 = CARTESIAN_POINT ( 'NONE',  ( -62.99999999999998579, 14.61458333265053611, 2.077350269189627952 ) ) ;
#2286 = VERTEX_POINT ( 'NONE', #10633 ) ;
#2287 = DIRECTION ( 'NONE',  ( -1.000000000000000000, 0.000000000000000000, 0.000000000000000000 ) ) ;
#2288 = DIRECTION ( 'NONE',  ( 0.000000000000000000, 0.000000000000000000, -1.000000000000000000 ) ) ;
#2289 = AXIS2_PLACEMENT_3D ( 'NONE', #6388, #4032, #5542 ) ;
#2290 = ORIENTED_EDGE ( 'NONE', *, *, #57, .F. ) ;
#2291 = DIRECTION ( 'NONE',  ( 0.000000000000000000, -1.000000000000000000, 0.000000000000000000 ) ) ;
#2292 = EDGE_CURVE ( 'NONE', #9531, #2234, #5579, .T. ) ;
#2293 = CARTESIAN_POINT ( 'NONE',  ( -61.13531646874998415, 13.32812499965860020, 1.500000000000002220 ) ) ;
#2294 = CARTESIAN_POINT ( 'NONE',  ( -62.86468353124999453, 10.45312499965860198, 1.500000000000002220 ) ) ;
#2295 = CARTESIAN_POINT ( 'NONE',  ( -60.99999999999998579, 14.52083333333333393, 0.9226497308103762673 ) ) ;
#2296 = CARTESIAN_POINT ( 'NONE',  ( -61.56765823437498852, 11.09895833299193590, 2.248837904296538515 ) ) ;
#2297 = CARTESIAN_POINT ( 'NONE',  ( -61.56765823437498142, 15.43229166632526805, 0.7511620957034663704 ) ) ;
#2298 = EDGE_CURVE ( 'NONE', #9621, #5032, #764, .T. ) ;
#2299 = AXIS2_PLACEMENT_3D ( 'NONE', #10134, #84, #3415 ) ;
#2300 = APPLICATION_PROTOCOL_DEFINITION ( 'draft international standard', 'automotive_design', 1998, #4853 ) ;
#2301 = DIRECTION ( 'NONE',  ( 0.000000000000000000, 0.000000000000000000, -1.000000000000000000 ) ) ;
#2302 = CARTESIAN_POINT ( 'NONE',  ( -61.13531646874998415, 8.369791666325268054, 1.999225269531026417 ) ) ;
#2303 = CARTESIAN_POINT ( 'NONE',  ( -61.99999999999997868, 10.31250000000000000, 0.5000000000000013323 ) ) ;
#2304 = ORIENTED_EDGE ( 'NONE', *, *, #4899, .T. ) ;
#2305 = LINE ( 'NONE', #3501, #2306 ) ;
#2306 = VECTOR ( 'NONE', #7793, 1000.000000000000000 ) ;
#2307 = AXIS2_PLACEMENT_3D ( 'NONE', #5193, #3646, #1706 ) ;
#2308 =( BOUNDED_CURVE ( )  B_SPLINE_CURVE ( 2, ( #4623, #9737, #2911, #9797, #3797, #3671, #8966, #8022, #3020 ),
 .UNSPECIFIED., .F., .T. ) 
 B_SPLINE_CURVE_WITH_KNOTS ( ( 3, 2, 2, 2, 3 ),
 ( 0.2578125000000000000, 0.2604166666666666852, 0.2656250000000000000, 0.2708333333333333148, 0.2734375000000000000 ),
 .UNSPECIFIED. ) 
 CURVE ( )  GEOMETRIC_REPRESENTATION_ITEM ( )  RATIONAL_B_SPLINE_CURVE ( ( 0.9330127018922194093, 0.9330127018922194093, 1.000000000000000000, 0.8660254037844387076, 1.000000000000000000, 0.8660254037844387076, 1.000000000000000000, 0.9330127018922194093, 0.9330127018922194093 ) ) 
 REPRESENTATION_ITEM ( '' )  );
#2309 = CARTESIAN_POINT ( 'NONE',  ( -61.13531646874998415, 13.57812499965860198, 1.500000000000002220 ) ) ;
#2310 = CARTESIAN_POINT ( 'NONE',  ( -62.86468353124998032, 9.432291666325268054, 1.000774730468978246 ) ) ;
#2311 = DIRECTION ( 'NONE',  ( -1.000000000000000000, -0.000000000000000000, -0.000000000000000000 ) ) ;
#2312 = ORIENTED_EDGE ( 'NONE', *, *, #5271, .F. ) ;
#2313 = CARTESIAN_POINT ( 'NONE',  ( -61.49999999999998579, 13.95833333333333215, 2.366025403784441927 ) ) ;
#2314 = CIRCLE ( 'NONE', #9227, 6.000000000000005329 ) ;
#2315 = CARTESIAN_POINT ( 'NONE',  ( -61.99999999999998579, 12.15624999931720396, 2.654700538379254571 ) ) ;
#2316 = EDGE_CURVE ( 'NONE', #1066, #6626, #8807, .T. ) ;
#2317 = CARTESIAN_POINT ( 'NONE',  ( -61.13531646874998415, 13.82812499965860198, 1.500000000000002220 ) ) ;
#2318 =( LENGTH_UNIT ( ) NAMED_UNIT ( * ) SI_UNIT ( .MILLI., .METRE. ) );
#2319 = ORIENTED_EDGE ( 'NONE', *, *, #2298, .F. ) ;
#2320 = CARTESIAN_POINT ( 'NONE',  ( -62.86468353124998032, 10.99479166632526628, 1.000774730468978246 ) ) ;
#2321 = CARTESIAN_POINT ( 'NONE',  ( 144.0000000000000284, 5.500000000000000000, 0.000000000000000000 ) ) ;
#2322 = CARTESIAN_POINT ( 'NONE',  ( -61.56765823437498142, 15.93229166632526628, 0.7511620957034663704 ) ) ;
#2323 = ORIENTED_EDGE ( 'NONE', *, *, #6378, .F. ) ;
#2324 = EDGE_CURVE ( 'NONE', #8781, #10687, #6561, .T. ) ;
#2325 = CYLINDRICAL_SURFACE ( 'NONE', #879, 0.9999999999999981126 ) ;
#2326 = ORIENTED_EDGE ( 'NONE', *, *, #4725, .T. ) ;
#2327 = CARTESIAN_POINT ( 'NONE',  ( -61.99999999999997868, 9.781249999317202182, 0.5000000000000013323 ) ) ;
#2328 = ADVANCED_FACE ( 'NONE', ( #299, #7976 ), #4736, .T. ) ;
#2329 = CARTESIAN_POINT ( 'NONE',  ( -61.49999999999998579, 9.791666666666667851, 0.6339745962155628467 ) ) ;
#2330 = DIRECTION ( 'NONE',  ( 0.000000000000000000, -0.000000000000000000, -1.000000000000000000 ) ) ;
#2331 = CARTESIAN_POINT ( 'NONE',  ( -61.99999999999998579, 11.68749999999999822, 2.500000000000002665 ) ) ;
#2332 = CARTESIAN_POINT ( 'NONE',  ( -61.73205080756886787, 8.301335450315370679, 0.5000000000000002220 ) ) ;
#2333 = DIRECTION ( 'NONE',  ( 0.000000000000000000, -5.421010862427519705E-17, 1.000000000000000000 ) ) ;
#2334 = CARTESIAN_POINT ( 'NONE',  ( -62.86468353124998742, 12.28645833299193413, 1.999225269531025972 ) ) ;
#2335 = DIRECTION ( 'NONE',  ( -1.000000000000000000, 0.000000000000000000, 0.000000000000000000 ) ) ;
#2336 = ORIENTED_EDGE ( 'NONE', *, *, #2709, .T. ) ;
#2337 = LINE ( 'NONE', #9118, #4782 ) ;
#2338 = ORIENTED_EDGE ( 'NONE', *, *, #3145, .F. ) ;
#2339 = CYLINDRICAL_SURFACE ( 'NONE', #1999, 0.9999999999999981126 ) ;
#2340 = CARTESIAN_POINT ( 'NONE',  ( -62.86468353124999453, 13.70312499965860198, 1.500000000000002220 ) ) ;
#2341 = DIRECTION ( 'NONE',  ( 0.000000000000000000, 0.000000000000000000, -1.000000000000000000 ) ) ;
#2342 = DIRECTION ( 'NONE',  ( 0.000000000000000000, 0.000000000000000000, -1.000000000000000000 ) ) ;
#2343 = VECTOR ( 'NONE', #8296, 1000.000000000000000 ) ;
#2344 = CARTESIAN_POINT ( 'NONE',  ( -62.86468353124998032, 11.74479166632526628, 1.000774730468978024 ) ) ;
#2345 = CARTESIAN_POINT ( 'NONE',  ( -62.86468353124998032, 15.49479166632526628, 1.000774730468978246 ) ) ;
#2346 = ITEM_DEFINED_TRANSFORMATION ( 'NONE', 'NONE', #5304,  #2307 ) ;
#2347 = FACE_OUTER_BOUND ( 'NONE', #7855, .T. ) ;
#2348 = CARTESIAN_POINT ( 'NONE',  ( -60.99999999999998579, 15.69791666598386648, 2.077350269189628840 ) ) ;
#2349 = DIRECTION ( 'NONE',  ( 0.000000000000000000, 0.000000000000000000, -1.000000000000000000 ) ) ;
#2350 = ORIENTED_EDGE ( 'NONE', *, *, #5232, .T. ) ;
#2351 = LINE ( 'NONE', #9970, #10146 ) ;
#2352 = AXIS2_PLACEMENT_3D ( 'NONE', #10029, #5915, #1583 ) ;
#2353 = VECTOR ( 'NONE', #4603, 1000.000000000000000 ) ;
#2354 = EDGE_CURVE ( 'NONE', #2668, #10100, #8829, .T. ) ;
#2355 = CARTESIAN_POINT ( 'NONE',  ( -61.99999999999999289, 14.51562499965860020, 2.498450539062049724 ) ) ;
#2356 = CARTESIAN_POINT ( 'NONE',  ( -61.99999999999998579, 10.39062499965860020, 0.5015494609379544944 ) ) ;
#2357 = CARTESIAN_POINT ( 'NONE',  ( -61.56765823437498852, 16.09895833299193768, 2.248837904296538515 ) ) ;
#2358 = DIRECTION ( 'NONE',  ( 1.000000000000000000, -0.000000000000000000, -0.000000000000000000 ) ) ;
#2359 = VERTEX_POINT ( 'NONE', #4159 ) ;
#2360 = CARTESIAN_POINT ( 'NONE',  ( -62.99999999999998579, 14.39583333333333570, 2.077350269189627952 ) ) ;
#2361 = CARTESIAN_POINT ( 'NONE',  ( -61.99999999999998579, 11.15624999931720218, 2.500000000000002665 ) ) ;
#2362 =( NAMED_UNIT ( * ) SI_UNIT ( $, .STERADIAN. ) SOLID_ANGLE_UNIT ( ) );
#2363 = UNCERTAINTY_MEASURE_WITH_UNIT (LENGTH_MEASURE( 1.000000000000000082E-05 ), #1638, 'distance_accuracy_value', 'NONE');
#2364 = AXIS2_PLACEMENT_3D ( 'NONE', #5632, #3863, #8096 ) ;
#2365 = CARTESIAN_POINT ( 'NONE',  ( -62.99999999999998579, 11.34374999931720218, 1.500000000000001998 ) ) ;
#2366 = DIRECTION ( 'NONE',  ( -1.000000000000000000, 0.000000000000000000, 0.000000000000000000 ) ) ;
#2367 =( BOUNDED_CURVE ( )  B_SPLINE_CURVE ( 2, ( #9224, #9115, #5772, #1607, #8183, #1504, #4153, #4778, #3168 ),
 .UNSPECIFIED., .F., .F. ) 
 B_SPLINE_CURVE_WITH_KNOTS ( ( 3, 2, 2, 2, 3 ),
 ( 0.1015624999999999722, 0.1041666666666666713, 0.1093750000000000000, 0.1145833333333333287, 0.1171875000000000278 ),
 .UNSPECIFIED. ) 
 CURVE ( )  GEOMETRIC_REPRESENTATION_ITEM ( )  RATIONAL_B_SPLINE_CURVE ( ( 0.9330127018922194093, 0.9330127018922186322, 1.000000000000000000, 0.8660254037844387076, 1.000000000000000000, 0.8660254037844387076, 1.000000000000000000, 0.9330127018922186322, 0.9330127018922194093 ) ) 
 REPRESENTATION_ITEM ( '' )  );
#2368 = VECTOR ( 'NONE', #2130, 1000.000000000000000 ) ;
#2369 = CARTESIAN_POINT ( 'NONE',  ( -61.13531646874998415, 13.59895833299193413, 1.000774730468978468 ) ) ;
#2370 = ORIENTED_EDGE ( 'NONE', *, *, #3516, .F. ) ;
#2371 = EDGE_CURVE ( 'NONE', #7362, #9156, #6641, .T. ) ;
#2372 = CARTESIAN_POINT ( 'NONE',  ( -62.86468353124998742, 11.53645833299193413, 1.999225269531025972 ) ) ;
#2373 = CARTESIAN_POINT ( 'NONE',  ( -61.13531646874998415, 16.11979166632526628, 1.999225269531026417 ) ) ;
#2374 = ORIENTED_EDGE ( 'NONE', *, *, #5254, .T. ) ;
#2375 = CARTESIAN_POINT ( 'NONE',  ( -61.99999999999998579, 8.937500000000001776, 2.500000000000002665 ) ) ;
#2376 = VERTEX_POINT ( 'NONE', #672 ) ;
#2377 = CARTESIAN_POINT ( 'NONE',  ( -62.49999999999998579, 9.885416665983870033, 2.366025403784441483 ) ) ;
#2378 = CARTESIAN_POINT ( 'NONE',  ( -60.99999999999998579, 10.00000000000000000, 1.500000000000002220 ) ) ;
#2379 = LINE ( 'NONE', #7496, #9200 ) ;
#2380 = CARTESIAN_POINT ( 'NONE',  ( -61.99999999999998579, 16.00000000000000000, 1.500000000000002220 ) ) ;
#2381 = CARTESIAN_POINT ( 'NONE',  ( -62.99999999999998579, 9.343749999317202182, 1.500000000000001998 ) ) ;
#2382 = CARTESIAN_POINT ( 'NONE',  ( -62.43234176562498305, 11.47395833299193590, 0.7511620957034662593 ) ) ;
#2383 = CARTESIAN_POINT ( 'NONE',  ( 0.000000000000000000, 0.000000000000000000, 3.000000000000000000 ) ) ;
#2384 = VERTEX_POINT ( 'NONE', #9281 ) ;
#2385 = DIRECTION ( 'NONE',  ( -0.000000000000000000, -0.000000000000000000, 1.000000000000000000 ) ) ;
#2386 = DIRECTION ( 'NONE',  ( -0.000000000000000000, -0.000000000000000000, 1.000000000000000000 ) ) ;
#2387 = DIRECTION ( 'NONE',  ( -1.000000000000000000, 0.000000000000000000, 0.000000000000000000 ) ) ;
#2388 = CARTESIAN_POINT ( 'NONE',  ( -62.86468353124998032, 14.18229166632526983, 1.000774730468978246 ) ) ;
#2389 = CARTESIAN_POINT ( 'NONE',  ( -61.99999999999998579, 13.81249999999999822, 0.5000000000000013323 ) ) ;
#2390 = CARTESIAN_POINT ( 'NONE',  ( -62.26794919243110371, 8.176335450315370679, 2.500000000000000888 ) ) ;
#2391 = CARTESIAN_POINT ( 'NONE',  ( -49.99999999999998579, -15.00000000000001243, 5.000000000000004441 ) ) ;
#2392 = CARTESIAN_POINT ( 'NONE',  ( -62.86468353124999453, 13.26562499965860198, 1.500000000000002220 ) ) ;
#2393 = CARTESIAN_POINT ( 'NONE',  ( -61.99999999999998579, 15.95312499965860198, 0.5015494609379544944 ) ) ;
#2394 = DIRECTION ( 'NONE',  ( 1.000000000000000000, 0.000000000000000000, 0.000000000000000000 ) ) ;
#2395 = CONTEXT_DEPENDENT_SHAPE_REPRESENTATION ( #5053, #5641 ) ;
#2396 = CARTESIAN_POINT ( 'NONE',  ( -62.26794919243111082, 13.64508544963257286, 2.500000000000003109 ) ) ;
#2397 = CARTESIAN_POINT ( 'NONE',  ( -60.99999999999998579, 15.71874999931720218, 1.500000000000002220 ) ) ;
#2398 = PLANE ( 'NONE',  #5534 ) ;
#2399 = ORIENTED_EDGE ( 'NONE', *, *, #10843, .T. ) ;
#2400 = FACE_OUTER_BOUND ( 'NONE', #5072, .T. ) ;
#2401 = EDGE_CURVE ( 'NONE', #2572, #8685, #3085, .T. ) ;
#2402 = DIRECTION ( 'NONE',  ( 0.000000000000000000, 0.000000000000000000, 1.000000000000000000 ) ) ;
#2403 = CARTESIAN_POINT ( 'NONE',  ( -61.13531646874997705, 13.59895833299193413, 1.000774730468978468 ) ) ;
#2404 = CARTESIAN_POINT ( 'NONE',  ( -62.43234176562498305, 9.411458332991935904, 0.7511620957034662593 ) ) ;
#2405 = CARTESIAN_POINT ( 'NONE',  ( -62.43234176562498305, 8.161458332991934128, 0.7511620957034662593 ) ) ;
#2406 = CARTESIAN_POINT ( 'NONE',  ( -61.99999999999998579, 16.00000000000000000, 2.500000000000000444 ) ) ;
#2407 = EDGE_LOOP ( 'NONE', ( #2965, #10037, #495, #3322 ) ) ;
#2408 = CARTESIAN_POINT ( 'NONE',  ( -62.99999999999998579, 13.64583333333333215, 2.077350269189627952 ) ) ;
#2409 = CARTESIAN_POINT ( 'NONE',  ( -61.56765823437498852, 9.348958332991935904, 2.248837904296538515 ) ) ;
#2410 = CARTESIAN_POINT ( 'NONE',  ( -60.99999999999998579, 11.71874999931720218, 1.500000000000002220 ) ) ;
#2411 = EDGE_CURVE ( 'NONE', #8509, #8229, #4059, .T. ) ;
#2412 = DIRECTION ( 'NONE',  ( -0.000000000000000000, -1.000000000000000000, -0.000000000000000000 ) ) ;
#2413 = CARTESIAN_POINT ( 'NONE',  ( -61.99999999999998579, 13.76562499965860020, 2.498450539062049724 ) ) ;
#2414 = CARTESIAN_POINT ( 'NONE',  ( -61.99999999999998579, 16.00000000000000000, 2.500000000000000444 ) ) ;
#2415 = ORIENTED_EDGE ( 'NONE', *, *, #7985, .T. ) ;
#2416 = ADVANCED_FACE ( 'NONE', ( #10891 ), #5779, .T. ) ;
#2417 = CARTESIAN_POINT ( 'NONE',  ( -62.86468353124998742, 11.03645833299193413, 1.999225269531025972 ) ) ;
#2418 = LINE ( 'NONE', #8374, #4937 ) ;
#2419 = EDGE_CURVE ( 'NONE', #3958, #3072, #6057, .T. ) ;
#2420 = DIRECTION ( 'NONE',  ( 0.000000000000000000, -1.224646799147352961E-16, 1.000000000000000000 ) ) ;
#2421 = ORIENTED_EDGE ( 'NONE', *, *, #3578, .T. ) ;
#2422 = CARTESIAN_POINT ( 'NONE',  ( -99.99999999999995737, -12.99999999999998757, 3.000000000000000000 ) ) ;
#2423 = EDGE_CURVE ( 'NONE', #9337, #5402, #10937, .T. ) ;
#2424 = PRODUCT_RELATED_PRODUCT_CATEGORY ( 'part', '', ( #3510 ) ) ;
#2425 = ORIENTED_EDGE ( 'NONE', *, *, #8312, .T. ) ;
#2426 = CARTESIAN_POINT ( 'NONE',  ( -78.99999999999998579, -11.50000000000000711, 5.000000000000000000 ) ) ;
#2427 = CARTESIAN_POINT ( 'NONE',  ( -62.99999999999998579, 10.87500000000000000, 1.500000000000001998 ) ) ;
#2428 = AXIS2_PLACEMENT_3D ( 'NONE', #6380, #8939, #3823 ) ;
#2429 = VERTEX_POINT ( 'NONE', #6630 ) ;
#2430 = CARTESIAN_POINT ( 'NONE',  ( -61.99999999999998579, 14.90624999931720218, 2.500000000000002665 ) ) ;
#2431 = CARTESIAN_POINT ( 'NONE',  ( -61.49999999999998579, 10.42708333265053611, 2.366025403784441927 ) ) ;
#2432 = CARTESIAN_POINT ( 'NONE',  ( -62.86468353124998742, 13.78645833299193235, 1.999225269531025972 ) ) ;
#2433 = PLANE ( 'NONE',  #7154 ) ;
#2434 = ORIENTED_EDGE ( 'NONE', *, *, #3464, .T. ) ;
#2435 = LINE ( 'NONE', #6624, #10095 ) ;
#2436 = EDGE_CURVE ( 'NONE', #4203, #4184, #3595, .T. ) ;
#2437 = AXIS2_PLACEMENT_3D ( 'NONE', #7643, #10183, #3463 ) ;
#2438 = ORIENTED_EDGE ( 'NONE', *, *, #10418, .F. ) ;
#2439 = DIRECTION ( 'NONE',  ( 0.000000000000000000, 1.000000000000000000, 0.000000000000000000 ) ) ;
#2440 = CARTESIAN_POINT ( 'NONE',  ( -61.99999999999998579, 15.14062499965860198, 0.5015494609379544944 ) ) ;
#2441 = DIRECTION ( 'NONE',  ( 1.000000000000000000, 0.000000000000000000, 0.000000000000000000 ) ) ;
#2442 =( LENGTH_UNIT ( ) NAMED_UNIT ( * ) SI_UNIT ( .MILLI., .METRE. ) );
#2443 = LINE ( 'NONE', #10688, #10954 ) ;
#2444 = CARTESIAN_POINT ( 'NONE',  ( -61.99999999999999289, 12.82812499965860198, 2.498450539062049724 ) ) ;
#2445 = VECTOR ( 'NONE', #7190, 1000.000000000000000 ) ;
#2446 = CARTESIAN_POINT ( 'NONE',  ( -62.86468353124998032, 15.24479166632526805, 1.000774730468978246 ) ) ;
#2447 = CARTESIAN_POINT ( 'NONE',  ( -139.9999999999999716, -8.000000000000000000, 0.000000000000000000 ) ) ;
#2448 = EDGE_CURVE ( 'NONE', #2594, #10259, #8769, .T. ) ;
#2449 = CARTESIAN_POINT ( 'NONE',  ( -61.49999999999998579, 13.42708333265053433, 2.366025403784441927 ) ) ;
#2450 = CARTESIAN_POINT ( 'NONE',  ( -61.56765823437498852, 9.598958332991934128, 2.248837904296538515 ) ) ;
#2451 = VECTOR ( 'NONE', #6937, 1000.000000000000000 ) ;
#2452 = CARTESIAN_POINT ( 'NONE',  ( -105.0000000000000000, 0.000000000000000000, 3.000000000000000000 ) ) ;
#2453 = ORIENTED_EDGE ( 'NONE', *, *, #10147, .F. ) ;
#2454 = CARTESIAN_POINT ( 'NONE',  ( -44.00000000000000000, -14.00000000000000888, -0.9999999999999947820 ) ) ;
#2455 = CARTESIAN_POINT ( 'NONE',  ( -120.0000000000000000, 8.000000000000000000, 0.000000000000000000 ) ) ;
#2456 =( BOUNDED_CURVE ( )  B_SPLINE_CURVE ( 2, ( #3426, #5821, #5197, #926, #9220, #8601, #8385, #6827, #4307 ),
 .UNSPECIFIED., .F., .F. ) 
 B_SPLINE_CURVE_WITH_KNOTS ( ( 3, 2, 2, 2, 3 ),
 ( 0.6953125000000000000, 0.6979166666666666297, 0.7031250000000000000, 0.7083333333333333703, 0.7109375000000000000 ),
 .UNSPECIFIED. ) 
 CURVE ( )  GEOMETRIC_REPRESENTATION_ITEM ( )  RATIONAL_B_SPLINE_CURVE ( ( 0.9330127018922194093, 0.9330127018922194093, 1.000000000000000000, 0.8660254037844387076, 1.000000000000000000, 0.8660254037844387076, 1.000000000000000000, 0.9330127018922194093, 0.9330127018922194093 ) ) 
 REPRESENTATION_ITEM ( '' )  );
#2457 = EDGE_CURVE ( 'NONE', #5442, #2721, #1122, .T. ) ;
#2458 = CONICAL_SURFACE ( 'NONE', #10080, 5.000000000000018652, 0.7853981633974430610 ) ;
#2459 = CARTESIAN_POINT ( 'NONE',  ( -61.13531646874997705, 14.05729166632526805, 1.999225269531026417 ) ) ;
#2460 = CARTESIAN_POINT ( 'NONE',  ( -62.43234176562498305, 11.16145833299193590, 0.7511620957034662593 ) ) ;
#2461 = CARTESIAN_POINT ( 'NONE',  ( -61.56765823437498142, 8.119791666325268054, 0.7511620957034663704 ) ) ;
#2462 = AXIS2_PLACEMENT_3D ( 'NONE', #7264, #4891, #10942 ) ;
#2463 = FACE_BOUND ( 'NONE', #6963, .T. ) ;
#2464 = ORIENTED_EDGE ( 'NONE', *, *, #4239, .T. ) ;
#2465 = CARTESIAN_POINT ( 'NONE',  ( -60.99999999999998579, 13.22916666666666607, 2.077350269189628840 ) ) ;
#2466 = EDGE_CURVE ( 'NONE', #6070, #847, #10155, .T. ) ;
#2467 = CARTESIAN_POINT ( 'NONE',  ( -61.99999999999999289, 8.203124999658601979, 0.5015494609379544944 ) ) ;
#2468 = SURFACE_SIDE_STYLE ('',( #7531 ) ) ;
#2469 = VECTOR ( 'NONE', #2735, 1000.000000000000000 ) ;
#2470 = CARTESIAN_POINT ( 'NONE',  ( -60.99999999999998579, 12.44791666598386826, 2.077350269189628840 ) ) ;
#2471 = VERTEX_POINT ( 'NONE', #830 ) ;
#2472 = CARTESIAN_POINT ( 'NONE',  ( -61.99999999999998579, -15.00000000000001421, 1.500000000000002220 ) ) ;
#2473 = MECHANICAL_DESIGN_GEOMETRIC_PRESENTATION_REPRESENTATION (  '', ( #7798 ), #539 ) ;
#2474 = CARTESIAN_POINT ( 'NONE',  ( -61.99999999999998579, 13.64062499965860198, 0.5015494609379544944 ) ) ;
#2475 = CARTESIAN_POINT ( 'NONE',  ( 0.000000000000000000, 0.000000000000000000, 0.000000000000000000 ) ) ;
#2476 = AXIS2_PLACEMENT_3D ( 'NONE', #1494, #6503, #3105 ) ;
#2477 = ORIENTED_EDGE ( 'NONE', *, *, #4906, .T. ) ;
#2478 = AXIS2_PLACEMENT_3D ( 'NONE', #6248, #3679, #4628 ) ;
#2479 = CARTESIAN_POINT ( 'NONE',  ( -62.86468353124998742, 12.28645833299193413, 1.999225269531025972 ) ) ;
#2480 = CARTESIAN_POINT ( 'NONE',  ( -61.99999999999998579, 16.15624999931720041, 2.500000000000002665 ) ) ;
#2481 = PRODUCT_DEFINITION_CONTEXT ( 'detailed design', #6495, 'design' ) ;
#2482 = AXIS2_PLACEMENT_3D ( 'NONE', #2422, #2591, #5928 ) ;
#2483 = CARTESIAN_POINT ( 'NONE',  ( 0.2309188673393134938, 0.2499999999999982792, 1.812888087824517713 ) ) ;
#2484 = ORIENTED_EDGE ( 'NONE', *, *, #7252, .T. ) ;
#2485 = CARTESIAN_POINT ( 'NONE',  ( -46.99999999999998579, -15.00000000000001066, 3.000000000000000000 ) ) ;
#2486 = ADVANCED_FACE ( 'NONE', ( #5941 ), #6580, .F. ) ;
#2487 = EDGE_CURVE ( 'NONE', #5990, #5765, #770, .T. ) ;
#2488 = ORIENTED_EDGE ( 'NONE', *, *, #6301, .T. ) ;
#2489 = CARTESIAN_POINT ( 'NONE',  ( -61.49999999999998579, 10.45833333333333393, 2.366025403784441927 ) ) ;
#2490 = ORIENTED_EDGE ( 'NONE', *, *, #8209, .T. ) ;
#2491 = CARTESIAN_POINT ( 'NONE',  ( -62.86468353124998742, 8.536458332991934128, 1.999225269531025972 ) ) ;
#2492 = DIRECTION ( 'NONE',  ( 0.000000000000000000, 0.000000000000000000, -1.000000000000000000 ) ) ;
#2493 = CARTESIAN_POINT ( 'NONE',  ( -62.86468353124998742, 13.53645833299193413, 1.999225269531025972 ) ) ;
#2494 = CARTESIAN_POINT ( 'NONE',  ( 150.0000000000000000, -8.000000000000000000, 6.000000000000000000 ) ) ;
#2495 = ORIENTED_EDGE ( 'NONE', *, *, #4924, .F. ) ;
#2496 = CARTESIAN_POINT ( 'NONE',  ( -61.99999999999998579, 9.312500000000000000, 0.5000000000000013323 ) ) ;
#2497 = EDGE_LOOP ( 'NONE', ( #2139, #10675, #9720 ) ) ;
#2498 = DIRECTION ( 'NONE',  ( 0.000000000000000000, 0.000000000000000000, -1.000000000000000000 ) ) ;
#2499 = CARTESIAN_POINT ( 'NONE',  ( -61.13531646874998415, 14.57812499965860020, 1.500000000000002220 ) ) ;
#2500 = CARTESIAN_POINT ( 'NONE',  ( -62.49999999999998579, 11.83333333333333215, 0.6339745962155627357 ) ) ;
#2501 = DIRECTION ( 'NONE',  ( 0.000000000000000000, 0.000000000000000000, 1.000000000000000000 ) ) ;
#2502 = DIRECTION ( 'NONE',  ( 0.000000000000000000, -0.000000000000000000, -1.000000000000000000 ) ) ;
#2503 = CARTESIAN_POINT ( 'NONE',  ( -61.99999999999999289, 13.32812499965860020, 2.498450539062049724 ) ) ;
#2504 = EDGE_CURVE ( 'NONE', #10287, #7557, #1560, .T. ) ;
#2505 = CARTESIAN_POINT ( 'NONE',  ( -61.13531646874998415, 15.91145833299193590, 1.000774730468978468 ) ) ;
#2506 = DIRECTION ( 'NONE',  ( 0.000000000000000000, 0.000000000000000000, -1.000000000000000000 ) ) ;
#2507 = DIRECTION ( 'NONE',  ( -0.000000000000000000, -0.000000000000000000, -1.000000000000000000 ) ) ;
#2508 = AXIS2_PLACEMENT_3D ( 'NONE', #10641, #10702, #2257 ) ;
#2509 = CARTESIAN_POINT ( 'NONE',  ( -61.56765823437498852, 8.848958332991934128, 2.248837904296538515 ) ) ;
#2510 = DIRECTION ( 'NONE',  ( 0.000000000000000000, -1.000000000000000000, 0.000000000000000000 ) ) ;
#2511 = EDGE_LOOP ( 'NONE', ( #1590, #7595, #1354, #8774 ) ) ;
#2512 = FACE_BOUND ( 'NONE', #4343, .T. ) ;
#2513 = CARTESIAN_POINT ( 'NONE',  ( -61.99999999999998579, 14.99999999999998579, 1.500000000000002220 ) ) ;
#2514 = CLOSED_SHELL ( 'NONE', ( #5138, #1519, #6235, #7428, #1408, #1814, #2328, #2854, #2804, #7177, #9480, #8967, #9873, #4092, #4117, #3301, #5550, #1107, #1948, #4029, #5963, #6423, #2784, #6008, #4487, #2181, #4923, #4555, #5342, #5724, #924, #10376, #9047, #2947, #5677, #3237, #20, #3957, #7646, #8158, #8848 ) ) ;
#2515 = CARTESIAN_POINT ( 'NONE',  ( -61.56765823437498852, 15.03645833299193590, 2.248837904296538515 ) ) ;
#2516 = CARTESIAN_POINT ( 'NONE',  ( -61.13531646874998415, 11.09895833299193413, 1.000774730468978468 ) ) ;
#2517 = CARTESIAN_POINT ( 'NONE',  ( -61.56765823437498142, 15.68229166632526628, 0.7511620957034663704 ) ) ;
#2518 = LINE ( 'NONE', #6693, #6429 ) ;
#2519 = ORIENTED_EDGE ( 'NONE', *, *, #6829, .T. ) ;
#2520 = CARTESIAN_POINT ( 'NONE',  ( -61.99999999999998579, 14.81250000000000000, 0.3452994616207497591 ) ) ;
#2521 = CARTESIAN_POINT ( 'NONE',  ( -62.43234176562499016, 8.807291666325268054, 2.248837904296538071 ) ) ;
#2522 = CARTESIAN_POINT ( 'NONE',  ( -61.99999999999998579, 13.40624999931720041, 2.654700538379254571 ) ) ;
#2523 = ORIENTED_EDGE ( 'NONE', *, *, #10862, .T. ) ;
#2524 =( BOUNDED_CURVE ( )  B_SPLINE_CURVE ( 2, ( #2160, #3148, #491, #4647, #9042, #1433, #550, #6546, #10653 ),
 .UNSPECIFIED., .F., .F. ) 
 B_SPLINE_CURVE_WITH_KNOTS ( ( 3, 2, 2, 2, 3 ),
 ( 0.8515625000000000000, 0.8541666666666666297, 0.8593750000000000000, 0.8645833333333333703, 0.8671875000000000000 ),
 .UNSPECIFIED. ) 
 CURVE ( )  GEOMETRIC_REPRESENTATION_ITEM ( )  RATIONAL_B_SPLINE_CURVE ( ( 0.9330127018922194093, 0.9330127018922194093, 1.000000000000000000, 0.8660254037844387076, 1.000000000000000000, 0.8660254037844387076, 1.000000000000000000, 0.9330127018922194093, 0.9330127018922194093 ) ) 
 REPRESENTATION_ITEM ( '' )  );
#2525=STYLED_ITEM('',(#11027),#1096);
#2526 = VECTOR ( 'NONE', #9527, 1000.000000000000000 ) ;
#2527 = ADVANCED_FACE ( 'NONE', ( #9231 ), #2606, .T. ) ;
#2528 = CARTESIAN_POINT ( 'NONE',  ( -62.86468353124998742, 13.47395833299193413, 1.999225269531025972 ) ) ;
#2529 = CARTESIAN_POINT ( 'NONE',  ( -49.99999999999998579, -14.00000000000001243, 83.15773105863907233 ) ) ;
#2530 = ORIENTED_EDGE ( 'NONE', *, *, #985, .T. ) ;
#2531 = VECTOR ( 'NONE', #3293, 1000.000000000000000 ) ;
#2532 = COLOUR_RGB ( '',1.000000000000000000, 0.9490196078431372140, 0.9098039215686274384 ) ;
#2533 = CARTESIAN_POINT ( 'NONE',  ( -61.13531646874998415, 13.11979166632526805, 1.999225269531026417 ) ) ;
#2534 = DIRECTION ( 'NONE',  ( -0.000000000000000000, -1.000000000000000000, -0.000000000000000000 ) ) ;
#2535 = EDGE_LOOP ( 'NONE', ( #10120, #10464, #891, #8479 ) ) ;
#2536 = DIRECTION ( 'NONE',  ( 0.9961946980917455452, 0.000000000000000000, -0.08715574274765831853 ) ) ;
#2537 = ORIENTED_EDGE ( 'NONE', *, *, #5651, .F. ) ;
#2538 = AXIS2_PLACEMENT_3D ( 'NONE', #5888, #3381, #8289 ) ;
#2539 = CARTESIAN_POINT ( 'NONE',  ( -62.49999999999998579, 12.41666666666666607, 2.366025403784441483 ) ) ;
#2540 = EDGE_CURVE ( 'NONE', #4509, #2018, #7211, .T. ) ;
#2541 = ORIENTED_EDGE ( 'NONE', *, *, #10681, .T. ) ;
#2542 = ORIENTED_EDGE ( 'NONE', *, *, #5180, .F. ) ;
#2543 = CARTESIAN_POINT ( 'NONE',  ( -61.99999999999998579, 8.953124999658601979, 0.5015494609379544944 ) ) ;
#2544 = LINE ( 'NONE', #5933, #5989 ) ;
#2545 = AXIS2_PLACEMENT_3D ( 'NONE', #1046, #9609, #5259 ) ;
#2546 = CARTESIAN_POINT ( 'NONE',  ( -61.99999999999998579, 13.82812499965860198, 2.498450539062049724 ) ) ;
#2547 = ADVANCED_FACE ( 'NONE', ( #6835 ), #8663, .T. ) ;
#2548 = CARTESIAN_POINT ( 'NONE',  ( 1.299999999999999156, 1.224646799147353207E-16, -1.000000000000000000 ) ) ;
#2549 = ORIENTED_EDGE ( 'NONE', *, *, #2298, .T. ) ;
#2550 = DIRECTION ( 'NONE',  ( -0.000000000000000000, -0.000000000000000000, -1.000000000000000000 ) ) ;
#2551 = ORIENTED_EDGE ( 'NONE', *, *, #466, .T. ) ;
#2552 = CARTESIAN_POINT ( 'NONE',  ( -61.99999999999997868, 11.65624999931720218, 2.500000000000002665 ) ) ;
#2553 = CARTESIAN_POINT ( 'NONE',  ( -62.86468353124998032, 15.68229166632526628, 1.000774730468978246 ) ) ;
#2554 = CARTESIAN_POINT ( 'NONE',  ( -60.99999999999998579, 13.77083333333333215, 0.9226497308103762673 ) ) ;
#2555 = CARTESIAN_POINT ( 'NONE',  ( -61.99999999999998579, 12.56249999999999822, 0.5000000000000013323 ) ) ;
#2556 = DIRECTION ( 'NONE',  ( 0.000000000000000000, 0.000000000000000000, -1.000000000000000000 ) ) ;
#2557 = CARTESIAN_POINT ( 'NONE',  ( -62.43234176562498305, 12.47395833299193413, 0.7511620957034662593 ) ) ;
#2558 = ADVANCED_BREP_SHAPE_REPRESENTATION ( '', ( #4773, #2307 ), #6215 ) ;
#2559 = CARTESIAN_POINT ( 'NONE',  ( -62.43234176562498305, 8.411458332991934128, 0.7511620957034662593 ) ) ;
#2560 = CARTESIAN_POINT ( 'NONE',  ( -49.99999999999998579, -15.00000000000001243, 4.000000000000003553 ) ) ;
#2561 = CARTESIAN_POINT ( 'NONE',  ( -51.99999999999999289, 3.184081677783117796E-15, 5.000000000000000000 ) ) ;
#2562 = CARTESIAN_POINT ( 'NONE',  ( -61.13531646874998415, 8.890624999658601979, 1.500000000000002220 ) ) ;
#2563 = DIRECTION ( 'NONE',  ( -0.000000000000000000, -0.000000000000000000, 1.000000000000000000 ) ) ;
#2564 = ORIENTED_EDGE ( 'NONE', *, *, #7874, .F. ) ;
#2565 = LINE ( 'NONE', #10273, #6018 ) ;
#2566 = DIRECTION ( 'NONE',  ( 1.000000000000000000, 0.000000000000000000, 0.000000000000000000 ) ) ;
#2567 = ADVANCED_FACE ( 'NONE', ( #104 ), #3489, .T. ) ;
#2568 = CARTESIAN_POINT ( 'NONE',  ( -62.86468353124999453, 15.47395833299193590, 1.999225269531025750 ) ) ;
#2569 = CARTESIAN_POINT ( 'NONE',  ( -61.56765823437498142, 10.86979166632526805, 0.7511620957034663704 ) ) ;
#2570 = CARTESIAN_POINT ( 'NONE',  ( -61.99999999999999289, 15.70312499965860198, 0.5015494609379544944 ) ) ;
#2571 = CARTESIAN_POINT ( 'NONE',  ( -61.99999999999998579, 14.99999999999998579, 0.5000000000000013323 ) ) ;
#2572 = VERTEX_POINT ( 'NONE', #4262 ) ;
#2573 = CARTESIAN_POINT ( 'NONE',  ( -61.49999999999998579, 14.54166666666666607, 0.6339745962155628467 ) ) ;
#2574 = CARTESIAN_POINT ( 'NONE',  ( -61.13531646874998415, 9.140624999658601979, 1.500000000000002220 ) ) ;
#2575 = CARTESIAN_POINT ( 'NONE',  ( -60.99999999999998579, 12.73958333265053611, 0.9226497308103762673 ) ) ;
#2576 = CARTESIAN_POINT ( 'NONE',  ( -62.99999999999998579, 14.64583333333333393, 2.077350269189627952 ) ) ;
#2577 = EDGE_LOOP ( 'NONE', ( #3816, #3576, #2818, #10901 ) ) ;
#2578 = FILL_AREA_STYLE_COLOUR ( '', #1101 ) ;
#2579 = CARTESIAN_POINT ( 'NONE',  ( -61.56765823437498852, 12.03645833299193413, 2.248837904296538515 ) ) ;
#2580 = SURFACE_STYLE_USAGE ( .BOTH. , #2695 ) ;
#2581 = VERTEX_POINT ( 'NONE', #2003 ) ;
#2582 = LINE ( 'NONE', #7392, #1491 ) ;
#2583 = CARTESIAN_POINT ( 'NONE',  ( -61.13531646874998415, 12.36979166632526628, 1.999225269531026417 ) ) ;
#2584 =( BOUNDED_CURVE ( )  B_SPLINE_CURVE ( 2, ( #3846, #2908, #8737, #5505, #7236, #7961, #7013, #1176, #7183 ),
 .UNSPECIFIED., .F., .T. ) 
 B_SPLINE_CURVE_WITH_KNOTS ( ( 3, 2, 2, 2, 3 ),
 ( 0.7109375000000000000, 0.7135416666666666297, 0.7187500000000000000, 0.7239583333333333703, 0.7265625000000000000 ),
 .UNSPECIFIED. ) 
 CURVE ( )  GEOMETRIC_REPRESENTATION_ITEM ( )  RATIONAL_B_SPLINE_CURVE ( ( 0.9330127018922194093, 0.9330127018922194093, 1.000000000000000000, 0.8660254037844387076, 1.000000000000000000, 0.8660254037844387076, 1.000000000000000000, 0.9330127018922194093, 0.9330127018922194093 ) ) 
 REPRESENTATION_ITEM ( '' )  );
#2585 = CYLINDRICAL_SURFACE ( 'NONE', #5657, 0.9999999999999981126 ) ;
#2586 = CARTESIAN_POINT ( 'NONE',  ( -60.99999999999998579, 8.947916665983870033, 2.077350269189628840 ) ) ;
#2587 = EDGE_CURVE ( 'NONE', #9263, #2273, #6891, .T. ) ;
#2588 = ORIENTED_EDGE ( 'NONE', *, *, #8038, .F. ) ;
#2589 = CARTESIAN_POINT ( 'NONE',  ( 140.0000000000000284, 8.000000000000000000, 3.000000000000000000 ) ) ;
#2590 = ORIENTED_EDGE ( 'NONE', *, *, #7696, .T. ) ;
#2591 = DIRECTION ( 'NONE',  ( -0.000000000000000000, -0.000000000000000000, 1.000000000000000000 ) ) ;
#2592 = ADVANCED_FACE ( 'NONE', ( #4491 ), #9437, .T. ) ;
#2593 = CARTESIAN_POINT ( 'NONE',  ( -61.13531646874998415, 11.84895833299193413, 1.000774730468978468 ) ) ;
#2594 = VERTEX_POINT ( 'NONE', #219 ) ;
#2595 = CARTESIAN_POINT ( 'NONE',  ( -61.56765823437498142, 8.432291666325268054, 0.7511620957034663704 ) ) ;
#2596 = CARTESIAN_POINT ( 'NONE',  ( -60.99999999999998579, 10.46874999931720218, 1.500000000000002220 ) ) ;
#2597 = EDGE_CURVE ( 'NONE', #5311, #3891, #7688, .T. ) ;
#2598 = SHAPE_DEFINITION_REPRESENTATION ( #4206, #5016 ) ;
#2599 = CARTESIAN_POINT ( 'NONE',  ( -61.13531646874998415, 12.64062499965860198, 1.500000000000002220 ) ) ;
#2600 = CARTESIAN_POINT ( 'NONE',  ( -62.49999999999998579, 12.80208333265053611, 0.6339745962155627357 ) ) ;
#2601 = ORIENTED_EDGE ( 'NONE', *, *, #2540, .T. ) ;
#2602 = FACE_BOUND ( 'NONE', #6294, .T. ) ;
#2603 = ORIENTED_EDGE ( 'NONE', *, *, #3545, .F. ) ;
#2604 = DIRECTION ( 'NONE',  ( -0.000000000000000000, -1.000000000000000000, -0.000000000000000000 ) ) ;
#2605 = CARTESIAN_POINT ( 'NONE',  ( -61.99999999999998579, 15.64062499965860198, 0.5015494609379544944 ) ) ;
#2606 = CYLINDRICAL_SURFACE ( 'NONE', #2028, 6.000000000000005329 ) ;
#2607 = CARTESIAN_POINT ( 'NONE',  ( -61.99999999999998579, 12.53124999931720396, 0.5000000000000013323 ) ) ;
#2608 = CARTESIAN_POINT ( 'NONE',  ( -62.99999999999998579, 12.36458333265053611, 2.077350269189627952 ) ) ;
#2609 = CARTESIAN_POINT ( 'NONE',  ( -61.56765823437498852, 14.59895833299193413, 2.248837904296538515 ) ) ;
#2610 = CARTESIAN_POINT ( 'NONE',  ( -61.13531646874998415, 8.828124999658601979, 1.500000000000002220 ) ) ;
#2611 = DIRECTION ( 'NONE',  ( -0.000000000000000000, -1.000000000000000000, -0.000000000000000000 ) ) ;
#2612 = CARTESIAN_POINT ( 'NONE',  ( -144.9999999999999716, 33.00000000000000000, 3.000000000000000000 ) ) ;
#2613 = CONICAL_SURFACE ( 'NONE', #7946, 23.99999999999999289, 0.7853981633974466137 ) ;
#2614 = CARTESIAN_POINT ( 'NONE',  ( -61.56765823437498852, 9.348958332991935904, 2.248837904296538515 ) ) ;
#2615 = CYLINDRICAL_SURFACE ( 'NONE', #1990, 0.9999999999999981126 ) ;
#2616 = EDGE_LOOP ( 'NONE', ( #5504, #1205, #2931, #6821 ) ) ;
#2617 = DIRECTION ( 'NONE',  ( 0.000000000000000000, -0.000000000000000000, -1.000000000000000000 ) ) ;
#2618 = CARTESIAN_POINT ( 'NONE',  ( -60.99999999999998579, 12.94791666598386826, 2.077350269189628840 ) ) ;
#2619 = EDGE_CURVE ( 'NONE', #10003, #386, #1945, .T. ) ;
#2620 = CARTESIAN_POINT ( 'NONE',  ( -61.13531646874997705, 15.55729166632526272, 1.999225269531026417 ) ) ;
#2621 = CARTESIAN_POINT ( 'NONE',  ( -62.43234176562498305, 10.91145833299193413, 0.7511620957034662593 ) ) ;
#2622 = ADVANCED_FACE ( 'NONE', ( #5207 ), #2841, .T. ) ;
#2623 = CARTESIAN_POINT ( 'NONE',  ( -61.13531646874998415, 9.328124999658600203, 1.500000000000002220 ) ) ;
#2624 = CARTESIAN_POINT ( 'NONE',  ( -61.99999999999998579, 13.15624999931720218, 2.500000000000002665 ) ) ;
#2625 = ORIENTED_EDGE ( 'NONE', *, *, #2056, .T. ) ;
#2626 = CARTESIAN_POINT ( 'NONE',  ( -62.99999999999998579, 15.39583333333333570, 2.077350269189627952 ) ) ;
#2627 = PRODUCT_DEFINITION_SHAPE ( 'NONE', 'NONE',  #10991 ) ;
#2628 = CARTESIAN_POINT ( 'NONE',  ( -62.43234176562499016, 8.557291666325268054, 2.248837904296538071 ) ) ;
#2629 = B_SPLINE_CURVE_WITH_KNOTS ( 'NONE', 3,
 ( #8617, #279, #1895, #2846, #1953, #10504 ),
 .UNSPECIFIED., .F., .F.,
 ( 4, 2, 4 ),
 ( 0.002363858439908545286, 0.002786031303543299881, 0.003208204167178054476 ),
 .UNSPECIFIED. ) ;
#2630 = AXIS2_PLACEMENT_3D ( 'NONE', #6401, #3064, #5609 ) ;
#2631 = DIRECTION ( 'NONE',  ( 0.000000000000000000, 0.000000000000000000, 1.000000000000000000 ) ) ;
#2632 = CARTESIAN_POINT ( 'NONE',  ( -62.49999999999998579, 13.38541666598387003, 2.366025403784441483 ) ) ;
#2633 = CARTESIAN_POINT ( 'NONE',  ( -62.49999999999998579, 14.66666666666666607, 2.366025403784441483 ) ) ;
#2634 = EDGE_LOOP ( 'NONE', ( #3642, #3317 ) ) ;
#2635 = CARTESIAN_POINT ( 'NONE',  ( -62.99999999999998579, 11.62500000000000000, 1.500000000000001998 ) ) ;
#2636 = CIRCLE ( 'NONE', #3165, 2.000000000000000000 ) ;
#2637 = VECTOR ( 'NONE', #5500, 1000.000000000000000 ) ;
#2638 = CARTESIAN_POINT ( 'NONE',  ( -61.56765823437498852, 11.78645833299193413, 2.248837904296538515 ) ) ;
#2639 = LINE ( 'NONE', #6025, #505 ) ;
#2640 = CARTESIAN_POINT ( 'NONE',  ( -60.99999999999998579, 15.50000000000000000, 1.500000000000002220 ) ) ;
#2641 = ORIENTED_EDGE ( 'NONE', *, *, #6974, .F. ) ;
#2642 = CARTESIAN_POINT ( 'NONE',  ( -62.49999999999998579, 12.83333333333333393, 0.6339745962155627357 ) ) ;
#2643 = VECTOR ( 'NONE', #7060, 1000.000000000000000 ) ;
#2644 = CARTESIAN_POINT ( 'NONE',  ( -62.86468353124999453, 12.26562499965860198, 1.500000000000002220 ) ) ;
#2645 = PRESENTATION_STYLE_ASSIGNMENT (( #970 ) ) ;
#2646 = LINE ( 'NONE', #6818, #1221 ) ;
#2647 = EDGE_CURVE ( 'NONE', #1405, #9106, #274, .T. ) ;
#2648 = CARTESIAN_POINT ( 'NONE',  ( -61.49999999999998579, 8.927083332650536107, 2.366025403784441927 ) ) ;
#2649 = COLOUR_RGB ( '',0.8941176470588234615, 0.8941176470588234615, 0.8941176470588234615 ) ;
#2650 = ORIENTED_EDGE ( 'NONE', *, *, #9461, .T. ) ;
#2651 = DIRECTION ( 'NONE',  ( 0.000000000000000000, 1.000000000000000000, 0.000000000000000000 ) ) ;
#2652 =( REPRESENTATION_RELATIONSHIP ('NONE','NONE', #560, #9271 ) REPRESENTATION_RELATIONSHIP_WITH_TRANSFORMATION ( #1769 )SHAPE_REPRESENTATION_RELATIONSHIP( ) );
#2653 = ORIENTED_EDGE ( 'NONE', *, *, #677, .F. ) ;
#2654 = CARTESIAN_POINT ( 'NONE',  ( -62.99999999999998579, 12.39583333333333393, 2.077350269189627952 ) ) ;
#2655 = VECTOR ( 'NONE', #8770, 1000.000000000000000 ) ;
#2656 = CARTESIAN_POINT ( 'NONE',  ( -61.99999999999998579, 11.64062499965860198, 0.5015494609379544944 ) ) ;
#2657 = ORIENTED_EDGE ( 'NONE', *, *, #6128, .F. ) ;
#2658 = CARTESIAN_POINT ( 'NONE',  ( -61.13531646874998415, 9.411458332991934128, 1.000774730468978468 ) ) ;
#2659 = CARTESIAN_POINT ( 'NONE',  ( -62.26794919243111082, 15.82366454968462932, 0.5000000000000013323 ) ) ;
#2660 = VECTOR ( 'NONE', #7626, 1000.000000000000000 ) ;
#2661 = EDGE_CURVE ( 'NONE', #8992, #506, #3982, .T. ) ;
#2662 = CARTESIAN_POINT ( 'NONE',  ( -61.99999999999998579, 13.32812499965860198, 2.498450539062049724 ) ) ;
#2663 = DIRECTION ( 'NONE',  ( 0.000000000000000000, -1.000000000000000000, 0.000000000000000000 ) ) ;
#2664 = CARTESIAN_POINT ( 'NONE',  ( -25.39999999999996305, 0.000000000000000000, 1.000000000000000000 ) ) ;
#2665 = ORIENTED_EDGE ( 'NONE', *, *, #9052, .F. ) ;
#2666 = CARTESIAN_POINT ( 'NONE',  ( -61.99999999999998579, 12.31249999999999822, 0.5000000000000013323 ) ) ;
#2667 = EDGE_CURVE ( 'NONE', #1175, #3747, #9383, .T. ) ;
#2668 = VERTEX_POINT ( 'NONE', #3437 ) ;
#2669 = CARTESIAN_POINT ( 'NONE',  ( -62.49999999999998579, 10.91666666666666607, 2.366025403784441483 ) ) ;
#2670 = CARTESIAN_POINT ( 'NONE',  ( -62.86468353124998742, 14.97395833299193590, 1.999225269531025972 ) ) ;
#2671 = CARTESIAN_POINT ( 'NONE',  ( -62.49999999999998579, 8.885416665983868256, 2.366025403784441483 ) ) ;
#2672 = DIRECTION ( 'NONE',  ( 0.000000000000000000, -0.000000000000000000, -1.000000000000000000 ) ) ;
#2673 = DIRECTION ( 'NONE',  ( 0.000000000000000000, -0.000000000000000000, 1.000000000000000000 ) ) ;
#2674 = CARTESIAN_POINT ( 'NONE',  ( -61.56765823437498852, 14.09895833299193413, 2.248837904296538515 ) ) ;
#2675 = CARTESIAN_POINT ( 'NONE',  ( -61.13531646874998415, 8.807291666325268054, 1.999225269531026417 ) ) ;
#2676 = LINE ( 'NONE', #5212, #1758 ) ;
#2677 = DIRECTION ( 'NONE',  ( -0.000000000000000000, -0.000000000000000000, -1.000000000000000000 ) ) ;
#2678 = CARTESIAN_POINT ( 'NONE',  ( -61.99999999999998579, 8.703124999658601979, 0.5015494609379544944 ) ) ;
#2679 = CARTESIAN_POINT ( 'NONE',  ( -61.99999999999998579, 15.78124999931720041, 0.5000000000000013323 ) ) ;
#2680 = VERTEX_POINT ( 'NONE', #5150 ) ;
#2681 = CARTESIAN_POINT ( 'NONE',  ( 0.5477065543514070267, 0.000000000000000000, 0.000000000000000000 ) ) ;
#2682 = CARTESIAN_POINT ( 'NONE',  ( -61.99999999999998579, -8.000000000000000000, 0.5000000000000013323 ) ) ;
#2683 = CARTESIAN_POINT ( 'NONE',  ( -61.56765823437498852, 15.53645833299193590, 2.248837904296538515 ) ) ;
#2684 = CARTESIAN_POINT ( 'NONE',  ( -62.86468353124998742, 10.72395833299193413, 1.999225269531025972 ) ) ;
#2685 = CARTESIAN_POINT ( 'NONE',  ( -62.86468353124999453, 8.703124999658601979, 1.500000000000002220 ) ) ;
#2686 = ORIENTED_EDGE ( 'NONE', *, *, #3107, .T. ) ;
#2687 = CARTESIAN_POINT ( 'NONE',  ( -61.99999999999998579, 15.56250000000000000, 0.3452994616207497591 ) ) ;
#2688 = CARTESIAN_POINT ( 'NONE',  ( -61.56765823437498142, 10.18229166632526805, 0.7511620957034663704 ) ) ;
#2689 = CARTESIAN_POINT ( 'NONE',  ( -60.99999999999998579, 13.46874999931720218, 1.500000000000002220 ) ) ;
#2690 = DIRECTION ( 'NONE',  ( -0.000000000000000000, 0.000000000000000000, -1.000000000000000000 ) ) ;
#2691 = ORIENTED_EDGE ( 'NONE', *, *, #2647, .T. ) ;
#2692 = CARTESIAN_POINT ( 'NONE',  ( -105.0000000000000000, -2.500000000000000000, 4.000000000000000000 ) ) ;
#2693 = EDGE_CURVE ( 'NONE', #4361, #5520, #1285, .T. ) ;
#2694 = CARTESIAN_POINT ( 'NONE',  ( -61.99999999999999289, 12.01562499965860198, 2.498450539062049724 ) ) ;
#2695 = SURFACE_SIDE_STYLE ('',( #907 ) ) ;
#2696 = CARTESIAN_POINT ( 'NONE',  ( -61.99999999999998579, 16.00000000000000000, 1.500000000000002220 ) ) ;
#2697 = ORIENTED_EDGE ( 'NONE', *, *, #7200, .F. ) ;
#2698 = CARTESIAN_POINT ( 'NONE',  ( -60.99999999999998579, 11.72916666666666607, 2.077350269189628840 ) ) ;
#2699 = DIRECTION ( 'NONE',  ( -0.000000000000000000, -1.000000000000000000, -0.000000000000000000 ) ) ;
#2700 = CARTESIAN_POINT ( 'NONE',  ( -61.13531646874998415, 14.89062499965860020, 1.500000000000002220 ) ) ;
#2701 = CARTESIAN_POINT ( 'NONE',  ( -61.73205080756886076, 10.30133545031537068, 0.5000000000000044409 ) ) ;
#2702 = VECTOR ( 'NONE', #385, 1000.000000000000000 ) ;
#2703 = CARTESIAN_POINT ( 'NONE',  ( -62.99999999999998579, 9.322916665983870033, 0.9226497308103756012 ) ) ;
#2704 = ORIENTED_EDGE ( 'NONE', *, *, #3929, .F. ) ;
#2705 = LINE ( 'NONE', #974, #3898 ) ;
#2706 = CARTESIAN_POINT ( 'NONE',  ( 1.299999999999999156, 2.449293598294706907E-16, 2.000000000000000000 ) ) ;
#2707 = VECTOR ( 'NONE', #10392, 1000.000000000000000 ) ;
#2708 = CARTESIAN_POINT ( 'NONE',  ( -62.43234176562498305, 10.91145833299193413, 0.7511620957034662593 ) ) ;
#2709 = EDGE_CURVE ( 'NONE', #5522, #10281, #7118, .T. ) ;
#2710 = CIRCLE ( 'NONE', #7852, 1.000000000000000000 ) ;
#2711 =( NAMED_UNIT ( * ) PLANE_ANGLE_UNIT ( ) SI_UNIT ( $, .RADIAN. ) );
#2712 = ORIENTED_EDGE ( 'NONE', *, *, #339, .F. ) ;
#2713 = CARTESIAN_POINT ( 'NONE',  ( -61.99999999999998579, 8.828124999658601979, 2.498450539062049724 ) ) ;
#2714 = PLANE ( 'NONE',  #683 ) ;
#2715 = VECTOR ( 'NONE', #6517, 1000.000000000000000 ) ;
#2716 = CARTESIAN_POINT ( 'NONE',  ( -62.86468353124998742, 15.03645833299193590, 1.999225269531025972 ) ) ;
#2717 = LINE ( 'NONE', #2664, #7849 ) ;
#2718 = ORIENTED_EDGE ( 'NONE', *, *, #5610, .T. ) ;
#2719 = CARTESIAN_POINT ( 'NONE',  ( -77.99999999999998579, 0.000000000000000000, 13.00000000000000178 ) ) ;
#2720 =( BOUNDED_CURVE ( )  B_SPLINE_CURVE ( 2, ( #10047, #9847, #5879, #4427, #6101, #5086, #6882, #5145, #5252 ),
 .UNSPECIFIED., .F., .F. ) 
 B_SPLINE_CURVE_WITH_KNOTS ( ( 3, 2, 2, 2, 3 ),
 ( 0.4765625000000000000, 0.4791666666666666852, 0.4843750000000000000, 0.4895833333333333148, 0.4921875000000000000 ),
 .UNSPECIFIED. ) 
 CURVE ( )  GEOMETRIC_REPRESENTATION_ITEM ( )  RATIONAL_B_SPLINE_CURVE ( ( 0.9330127018922194093, 0.9330127018922194093, 1.000000000000000000, 0.8660254037844387076, 1.000000000000000000, 0.8660254037844387076, 1.000000000000000000, 0.9330127018922194093, 0.9330127018922194093 ) ) 
 REPRESENTATION_ITEM ( '' )  );
#2721 = VERTEX_POINT ( 'NONE', #9785 ) ;
#2722 = AXIS2_PLACEMENT_3D ( 'NONE', #618, #6864, #3357 ) ;
#2723 = FACE_OUTER_BOUND ( 'NONE', #2910, .T. ) ;
#2724 = CARTESIAN_POINT ( 'NONE',  ( -61.99999999999998579, 8.687500000000001776, 2.654700538379254571 ) ) ;
#2725 = DIRECTION ( 'NONE',  ( -1.000000000000000000, 0.000000000000000000, 0.000000000000000000 ) ) ;
#2726 = LINE ( 'NONE', #4435, #7598 ) ;
#2727 = CARTESIAN_POINT ( 'NONE',  ( -62.99999999999998579, 12.34374999931720218, 1.500000000000001998 ) ) ;
#2728 = CARTESIAN_POINT ( 'NONE',  ( -61.13531646874997705, 13.86979166632526628, 1.999225269531026417 ) ) ;
#2729 = CARTESIAN_POINT ( 'NONE',  ( -61.56765823437498852, 8.786458332991934128, 2.248837904296538515 ) ) ;
#2730 = DIRECTION ( 'NONE',  ( 0.000000000000000000, 0.000000000000000000, -1.000000000000000000 ) ) ;
#2731 = CARTESIAN_POINT ( 'NONE',  ( -62.49999999999998579, 9.666666666666667851, 2.366025403784441483 ) ) ;
#2732 = CARTESIAN_POINT ( 'NONE',  ( -62.86468353124999453, 10.26562499965860198, 1.500000000000002220 ) ) ;
#2733 = CARTESIAN_POINT ( 'NONE',  ( -61.99999999999998579, 16.00000000000000000, 1.500000000000002220 ) ) ;
#2734 = VERTEX_POINT ( 'NONE', #6508 ) ;
#2735 = DIRECTION ( 'NONE',  ( -0.000000000000000000, -1.000000000000000000, -0.000000000000000000 ) ) ;
#2736 = FACE_OUTER_BOUND ( 'NONE', #8415, .T. ) ;
#2737 = CARTESIAN_POINT ( 'NONE',  ( -61.13531646874997705, 15.34895833299193590, 1.000774730468978468 ) ) ;
#2738 = CARTESIAN_POINT ( 'NONE',  ( -61.56765823437498852, 12.78645833299193413, 2.248837904296538515 ) ) ;
#2739 = CARTESIAN_POINT ( 'NONE',  ( -62.86468353124998032, 9.182291666325268054, 1.000774730468978024 ) ) ;
#2740 = CARTESIAN_POINT ( 'NONE',  ( -62.26794919243111082, 13.04241454900183328, 0.5000000000000013323 ) ) ;
#2741 = EDGE_LOOP ( 'NONE', ( #7713, #2014, #10651, #2858, #898, #271, #7934, #2149 ) ) ;
#2742 = CARTESIAN_POINT ( 'NONE',  ( -61.99999999999998579, 15.43750000000000000, 2.654700538379254571 ) ) ;
#2743 = CARTESIAN_POINT ( 'NONE',  ( -61.99999999999999289, 9.828124999658601979, 2.498450539062049724 ) ) ;
#2744 = CARTESIAN_POINT ( 'NONE',  ( -62.86468353124998742, 15.47395833299193413, 1.999225269531025972 ) ) ;
#2745 = EDGE_CURVE ( 'NONE', #1260, #6260, #2060, .T. ) ;
#2746 = CARTESIAN_POINT ( 'NONE',  ( -61.99999999999998579, 13.28124999931720396, 0.3452994616207497591 ) ) ;
#2747 = DIRECTION ( 'NONE',  ( -1.000000000000000000, -0.000000000000000000, -0.000000000000000000 ) ) ;
#2748 = EDGE_LOOP ( 'NONE', ( #7649, #3570, #5654, #3760 ) ) ;
#2749 = CARTESIAN_POINT ( 'NONE',  ( 144.0000000000000284, 5.500000000000000000, 3.000000000000000000 ) ) ;
#2750 = CARTESIAN_POINT ( 'NONE',  ( -62.43234176562498305, 11.41145833299193590, 0.7511620957034662593 ) ) ;
#2751 = DIRECTION ( 'NONE',  ( 1.000000000000000000, 0.000000000000000000, 0.000000000000000000 ) ) ;
#2752 = SHAPE_REPRESENTATION ( 'slotted pan head screw_iso_ISO 1580 - M2 x 6 - 6N', ( #2307 ), #4612 ) ;
#2753 = CARTESIAN_POINT ( 'NONE',  ( -60.99999999999998579, 15.52083333333333215, 0.9226497308103762673 ) ) ;
#2754 = VERTEX_POINT ( 'NONE', #565 ) ;
#2755 = CARTESIAN_POINT ( 'NONE',  ( -61.99999999999998579, 10.43750000000000178, 2.654700538379254571 ) ) ;
#2756 = CARTESIAN_POINT ( 'NONE',  ( -62.26794919243111082, 10.07366454968462932, 0.5000000000000013323 ) ) ;
#2757 = CARTESIAN_POINT ( 'NONE',  ( -61.13531646874998415, 13.61979166632526983, 1.999225269531026417 ) ) ;
#2758 = CARTESIAN_POINT ( 'NONE',  ( -61.99999999999998579, 11.06250000000000000, 0.5000000000000013323 ) ) ;
#2759 = CARTESIAN_POINT ( 'NONE',  ( -62.49999999999998579, 8.802083332650536107, 0.6339745962155627357 ) ) ;
#2760 = ORIENTED_EDGE ( 'NONE', *, *, #10476, .T. ) ;
#2761 = DIRECTION ( 'NONE',  ( -0.000000000000000000, 1.000000000000000000, -0.000000000000000000 ) ) ;
#2762 = CARTESIAN_POINT ( 'NONE',  ( -61.99999999999998579, 10.89062499965860020, 0.5015494609379544944 ) ) ;
#2763 = EDGE_CURVE ( 'NONE', #2359, #4541, #1235, .T. ) ;
#2764 = PRESENTATION_STYLE_ASSIGNMENT (( #5139 ) ) ;
#2765 = EDGE_LOOP ( 'NONE', ( #10564, #10658, #6014, #824 ) ) ;
#2766 = EDGE_CURVE ( 'NONE', #1066, #1268, #26, .T. ) ;
#2767 = CARTESIAN_POINT ( 'NONE',  ( -61.56765823437498142, 9.932291666325268054, 0.7511620957034663704 ) ) ;
#2768 = CARTESIAN_POINT ( 'NONE',  ( -57.99999999999998579, -10.00000000000000888, 3.000000000000000000 ) ) ;
#2769 = ADVANCED_FACE ( 'NONE', ( #8955 ), #8899, .T. ) ;
#2770 = CARTESIAN_POINT ( 'NONE',  ( -61.13531646874998415, 15.14062499965860020, 1.500000000000002220 ) ) ;
#2771 = DIRECTION ( 'NONE',  ( -0.000000000000000000, -1.000000000000000000, -0.000000000000000000 ) ) ;
#2772 = ORIENTED_EDGE ( 'NONE', *, *, #10211, .F. ) ;
#2773 = CARTESIAN_POINT ( 'NONE',  ( -61.99999999999998579, 16.00000000000000000, 2.500000000000000444 ) ) ;
#2774 = ORIENTED_EDGE ( 'NONE', *, *, #412, .T. ) ;
#2775 = CARTESIAN_POINT ( 'NONE',  ( -61.73205080756886076, 12.77008544963256931, 0.5000000000000014433 ) ) ;
#2776 = CARTESIAN_POINT ( 'NONE',  ( -60.99999999999998579, 8.979166666666666075, 2.077350269189628840 ) ) ;
#2777 = CARTESIAN_POINT ( 'NONE',  ( -62.99999999999998579, 9.895833333333333925, 2.077350269189627952 ) ) ;
#2778 = LINE ( 'NONE', #1946, #10799 ) ;
#2779 = CARTESIAN_POINT ( 'NONE',  ( -61.99999999999998579, 16.00000000000000000, 1.500000000000002220 ) ) ;
#2780 = CARTESIAN_POINT ( 'NONE',  ( -61.13531646874997705, 14.61979166632526805, 1.999225269531026417 ) ) ;
#2781 = CARTESIAN_POINT ( 'NONE',  ( -61.56765823437498142, 9.369791666325268054, 0.7511620957034663704 ) ) ;
#2782 = DIRECTION ( 'NONE',  ( 0.000000000000000000, 0.000000000000000000, -1.000000000000000000 ) ) ;
#2783 = CARTESIAN_POINT ( 'NONE',  ( -61.99999999999998579, 14.56249999999999822, 0.5000000000000013323 ) ) ;
#2784 = ADVANCED_FACE ( 'NONE', ( #3780 ), #7228, .T. ) ;
#2785 = CARTESIAN_POINT ( 'NONE',  ( -61.56765823437498852, 10.59895833299193413, 2.248837904296538515 ) ) ;
#2786 = LINE ( 'NONE', #5104, #9426 ) ;
#2787 = ORIENTED_EDGE ( 'NONE', *, *, #175, .T. ) ;
#2788 = CARTESIAN_POINT ( 'NONE',  ( 0.000000000000000000, 0.000000000000000000, 5.000000000000000000 ) ) ;
#2789 = CARTESIAN_POINT ( 'NONE',  ( -62.99999999999998579, 11.35416666666666607, 0.9226497308103756012 ) ) ;
#2790 = LINE ( 'NONE', #1123, #3238 ) ;
#2791 = CARTESIAN_POINT ( 'NONE',  ( -61.56765823437498142, 12.36979166632526805, 0.7511620957034663704 ) ) ;
#2792 = CARTESIAN_POINT ( 'NONE',  ( -62.43234176562498305, 8.411458332991934128, 0.7511620957034662593 ) ) ;
#2793 = EDGE_CURVE ( 'NONE', #4184, #353, #7173, .T. ) ;
#2794 = FACE_OUTER_BOUND ( 'NONE', #4485, .T. ) ;
#2795 = ORIENTED_EDGE ( 'NONE', *, *, #8073, .T. ) ;
#2796 = CARTESIAN_POINT ( 'NONE',  ( -62.99999999999998579, 10.84374999931720218, 1.500000000000001998 ) ) ;
#2797 = CARTESIAN_POINT ( 'NONE',  ( -62.86468353124998032, 10.49479166632526983, 1.000774730468978024 ) ) ;
#2798 = AXIS2_PLACEMENT_3D ( 'NONE', #8052, #8213, #603 ) ;
#2799 =( NAMED_UNIT ( * ) SI_UNIT ( $, .STERADIAN. ) SOLID_ANGLE_UNIT ( ) );
#2800 = CARTESIAN_POINT ( 'NONE',  ( -61.99999999999998579, 15.64062499965860198, 0.5015494609379544944 ) ) ;
#2801 = CARTESIAN_POINT ( 'NONE',  ( -61.49999999999998579, 14.42708333265053611, 2.366025403784441927 ) ) ;
#2802 = CYLINDRICAL_SURFACE ( 'NONE', #5740, 3.000000000000002665 ) ;
#2803 = ORIENTED_EDGE ( 'NONE', *, *, #3149, .F. ) ;
#2804 = ADVANCED_FACE ( 'NONE', ( #4714 ), #3062, .F. ) ;
#2805 = CARTESIAN_POINT ( 'NONE',  ( -25.39999999999996305, 0.000000000000000000, 1.000000000000000000 ) ) ;
#2806 = AXIS2_PLACEMENT_3D ( 'NONE', #6053, #5943, #2556 ) ;
#2807 = CARTESIAN_POINT ( 'NONE',  ( -62.86468353124999453, 11.47395833299193590, 1.999225269531025750 ) ) ;
#2808 = EDGE_CURVE ( 'NONE', #2208, #10486, #3720, .T. ) ;
#2809 = CARTESIAN_POINT ( 'NONE',  ( -62.86468353124998742, 8.223958332991934128, 1.999225269531025972 ) ) ;
#2810 = CARTESIAN_POINT ( 'NONE',  ( 195.0000000000000000, -2.500000000000000000, 4.000000000000000000 ) ) ;
#2811 = ORIENTED_EDGE ( 'NONE', *, *, #3578, .F. ) ;
#2812 = CARTESIAN_POINT ( 'NONE',  ( -62.49999999999998579, 12.58333333333333393, 0.6339745962155627357 ) ) ;
#2813 = DIRECTION ( 'NONE',  ( -0.000000000000000000, -1.000000000000000000, -0.000000000000000000 ) ) ;
#2814 = CARTESIAN_POINT ( 'NONE',  ( -62.86468353124998742, 13.78645833299193235, 1.999225269531025972 ) ) ;
#2815 = DIRECTION ( 'NONE',  ( 0.000000000000000000, 0.000000000000000000, -1.000000000000000000 ) ) ;
#2816 =( GEOMETRIC_REPRESENTATION_CONTEXT ( 3 ) GLOBAL_UNCERTAINTY_ASSIGNED_CONTEXT ( ( #6289 ) ) GLOBAL_UNIT_ASSIGNED_CONTEXT ( ( #4680, #9684, #5449 ) ) REPRESENTATION_CONTEXT ( 'NONE', 'WORKASPACE' ) );
#2817 = CARTESIAN_POINT ( 'NONE',  ( -61.99999999999998579, 10.28124999931720218, 0.3452994616207497591 ) ) ;
#2818 = ORIENTED_EDGE ( 'NONE', *, *, #3260, .T. ) ;
#2819 = CARTESIAN_POINT ( 'NONE',  ( -57.99999999999998579, -10.00000000000000888, 0.000000000000000000 ) ) ;
#2820 = AXIS2_PLACEMENT_3D ( 'NONE', #3839, #6229, #4493 ) ;
#2821 = CARTESIAN_POINT ( 'NONE',  ( -61.99999999999998579, 13.31249999999999822, 0.5000000000000013323 ) ) ;
#2822 =( BOUNDED_CURVE ( )  B_SPLINE_CURVE ( 2, ( #4759, #444, #3828, #8167, #7218, #557, #3102, #9259, #9309 ),
 .UNSPECIFIED., .F., .F. ) 
 B_SPLINE_CURVE_WITH_KNOTS ( ( 3, 2, 2, 2, 3 ),
 ( 0.5390625000000000000, 0.5416666666666666297, 0.5468750000000000000, 0.5520833333333333703, 0.5546875000000000000 ),
 .UNSPECIFIED. ) 
 CURVE ( )  GEOMETRIC_REPRESENTATION_ITEM ( )  RATIONAL_B_SPLINE_CURVE ( ( 0.9330127018922194093, 0.9330127018922194093, 1.000000000000000000, 0.8660254037844387076, 1.000000000000000000, 0.8660254037844387076, 1.000000000000000000, 0.9330127018922194093, 0.9330127018922194093 ) ) 
 REPRESENTATION_ITEM ( '' )  );
#2823 = CARTESIAN_POINT ( 'NONE',  ( -62.86468353124998742, 11.47395833299193590, 1.999225269531025972 ) ) ;
#2824 = FILL_AREA_STYLE_COLOUR ( '', #7051 ) ;
#2825 = AXIS2_PLACEMENT_3D ( 'NONE', #4035, #6451, #6557 ) ;
#2826 = ORIENTED_EDGE ( 'NONE', *, *, #9859, .F. ) ;
#2827 = VECTOR ( 'NONE', #7514, 999.9999999999998863 ) ;
#2828 = CARTESIAN_POINT ( 'NONE',  ( -62.43234176562499016, 10.30729166632526983, 2.248837904296538071 ) ) ;
#2829 = CARTESIAN_POINT ( 'NONE',  ( -49.99999999999998579, 8.000000000000001776, 83.15773105863907233 ) ) ;
#2830 = EDGE_CURVE ( 'NONE', #9377, #9531, #510, .T. ) ;
#2831 = VECTOR ( 'NONE', #9134, 1000.000000000000000 ) ;
#2832 = CARTESIAN_POINT ( 'NONE',  ( -61.99999999999998579, 14.57812499965860198, 2.498450539062049724 ) ) ;
#2833 = DIRECTION ( 'NONE',  ( 1.110223024625156540E-15, -1.000000000000000000, -0.000000000000000000 ) ) ;
#2834 = ORIENTED_EDGE ( 'NONE', *, *, #7357, .T. ) ;
#2835 = CARTESIAN_POINT ( 'NONE',  ( -61.99999999999998579, 9.437499999999998224, 2.500000000000002665 ) ) ;
#2836 = EDGE_CURVE ( 'NONE', #7251, #5256, #332, .T. ) ;
#2837 = VERTEX_POINT ( 'NONE', #3894 ) ;
#2838 = CARTESIAN_POINT ( 'NONE',  ( -61.99999999999998579, 16.00000000000000000, 1.500000000000002220 ) ) ;
#2839 = CARTESIAN_POINT ( 'NONE',  ( -61.99999999999998579, 9.062500000000000000, 0.3452994616207497591 ) ) ;
#2840 = AXIS2_PLACEMENT_3D ( 'NONE', #2788, #7066, #5389 ) ;
#2841 = CYLINDRICAL_SURFACE ( 'NONE', #9291, 0.9999999999999981126 ) ;
#2842 = CARTESIAN_POINT ( 'NONE',  ( 140.0000000000000568, 2.500000000000000000, 4.000000000000000000 ) ) ;
#2843 = CARTESIAN_POINT ( 'NONE',  ( -61.73205080756886076, 10.77008544963257286, 0.5000000000000014433 ) ) ;
#2844 = CARTESIAN_POINT ( 'NONE',  ( -61.56765823437498142, 13.68229166632526805, 0.7511620957034663704 ) ) ;
#2845 = CARTESIAN_POINT ( 'NONE',  ( -61.56765823437498852, 9.786458332991934128, 2.248837904296538515 ) ) ;
#2846 = CARTESIAN_POINT ( 'NONE',  ( 0.05007509226404534275, 0.2499999999999998335, 1.595201548406556036 ) ) ;
#2847 = CARTESIAN_POINT ( 'NONE',  ( -61.99999999999998579, 9.953124999658601979, 0.5015494609379544944 ) ) ;
#2848 = LINE ( 'NONE', #10615, #9097 ) ;
#2849 = ORIENTED_EDGE ( 'NONE', *, *, #1281, .F. ) ;
#2850 = DIRECTION ( 'NONE',  ( 0.000000000000000000, -0.000000000000000000, -1.000000000000000000 ) ) ;
#2851 = CARTESIAN_POINT ( 'NONE',  ( -61.99999999999998579, 15.31250000000000000, 0.5000000000000013323 ) ) ;
#2852 = CONICAL_SURFACE ( 'NONE', #3364, 1.000000000000000888, 1.029744259999999967 ) ;
#2853 = CARTESIAN_POINT ( 'NONE',  ( -61.49999999999998579, 15.79166666666666607, 0.6339745962155628467 ) ) ;
#2854 = ADVANCED_FACE ( 'NONE', ( #6459, #5607 ), #8177, .F. ) ;
#2855 = CARTESIAN_POINT ( 'NONE',  ( -61.99999999999998579, 13.01562499965860198, 2.498450539062049724 ) ) ;
#2856 = CARTESIAN_POINT ( 'NONE',  ( -61.99999999999999289, 9.015624999658601979, 2.498450539062049724 ) ) ;
#2857 = CARTESIAN_POINT ( 'NONE',  ( -62.26794919243110371, 8.573664549684629321, 0.4999999999999990563 ) ) ;
#2858 = ORIENTED_EDGE ( 'NONE', *, *, #1332, .T. ) ;
#2859 = CARTESIAN_POINT ( 'NONE',  ( -60.99999999999998579, 16.00000000000000000, 1.500000000000002220 ) ) ;
#2860 = CARTESIAN_POINT ( 'NONE',  ( -61.56765823437498852, 9.848958332991934128, 2.248837904296538515 ) ) ;
#2861 = PRODUCT_CONTEXT ( 'NONE', #10669, 'mechanical' ) ;
#2862 = CARTESIAN_POINT ( 'NONE',  ( -61.99999999999998579, 15.26562499965860020, 2.498450539062049724 ) ) ;
#2863 = CARTESIAN_POINT ( 'NONE',  ( -61.49999999999998579, 14.01041666598387003, 0.6339745962155628467 ) ) ;
#2864 = CARTESIAN_POINT ( 'NONE',  ( -61.99999999999998579, 8.187500000000001776, 2.500000000000003109 ) ) ;
#2865 = ORIENTED_EDGE ( 'NONE', *, *, #5787, .F. ) ;
#2866 = CARTESIAN_POINT ( 'NONE',  ( -62.99999999999998579, 11.64583333333333748, 2.077350269189627952 ) ) ;
#2867 = ORIENTED_EDGE ( 'NONE', *, *, #2540, .F. ) ;
#2868 = CARTESIAN_POINT ( 'NONE',  ( -62.43234176562499016, 12.99479166632526805, 2.248837904296538071 ) ) ;
#2869 = CARTESIAN_POINT ( 'NONE',  ( -62.86468353124999453, 8.953124999658601979, 1.500000000000002220 ) ) ;
#2870 = CYLINDRICAL_SURFACE ( 'NONE', #2508, 1.000000000000000888 ) ;
#2871 = ORIENTED_EDGE ( 'NONE', *, *, #2763, .F. ) ;
#2872 = CARTESIAN_POINT ( 'NONE',  ( -61.49999999999998579, 12.54166666666666607, 0.6339745962155628467 ) ) ;
#2873 = CARTESIAN_POINT ( 'NONE',  ( -61.99999999999998579, 16.00000000000000000, 2.500000000000000444 ) ) ;
#2874 = CARTESIAN_POINT ( 'NONE',  ( -61.13531646874998415, 14.86979166632526805, 1.999225269531026417 ) ) ;
#2875 = CARTESIAN_POINT ( 'NONE',  ( -61.99999999999997868, 10.31250000000000000, 0.5000000000000013323 ) ) ;
#2876 = CARTESIAN_POINT ( 'NONE',  ( -62.99999999999998579, 10.59374999931720396, 1.500000000000001998 ) ) ;
#2877 = ORIENTED_EDGE ( 'NONE', *, *, #10783, .T. ) ;
#2878 = VECTOR ( 'NONE', #10856, 1000.000000000000000 ) ;
#2879 = FACE_OUTER_BOUND ( 'NONE', #10873, .T. ) ;
#2880 = CARTESIAN_POINT ( 'NONE',  ( -49.99999999999998579, -14.00000000000001243, 3.000000000000000000 ) ) ;
#2881 = CARTESIAN_POINT ( 'NONE',  ( -61.13531646874998415, 12.32812499965860198, 1.500000000000002220 ) ) ;
#2882 = DIRECTION ( 'NONE',  ( 0.000000000000000000, 0.000000000000000000, -1.000000000000000000 ) ) ;
#2883 = ORIENTED_EDGE ( 'NONE', *, *, #3905, .T. ) ;
#2884 = AXIS2_PLACEMENT_3D ( 'NONE', #4167, #4122, #6532 ) ;
#2885 = CARTESIAN_POINT ( 'NONE',  ( -62.86468353124999453, 10.76562499965860020, 1.500000000000002220 ) ) ;
#2886 = FACE_OUTER_BOUND ( 'NONE', #10491, .T. ) ;
#2887 = EDGE_CURVE ( 'NONE', #1698, #2376, #4857, .T. ) ;
#2888 = CARTESIAN_POINT ( 'NONE',  ( -61.56765823437498142, 14.18229166632526805, 0.7511620957034663704 ) ) ;
#2889 = DIRECTION ( 'NONE',  ( 0.000000000000000000, 0.000000000000000000, -1.000000000000000000 ) ) ;
#2890 = ORIENTED_EDGE ( 'NONE', *, *, #4244, .F. ) ;
#2891 =( BOUNDED_SURFACE ( )  B_SPLINE_SURFACE ( 1, 2, ( 
 ( #4823, #619, #3163, #5713, #4044, #7446, #5035, #10928, #4199, #3479, #4252, #10093, #7657, #151, #2595, #6717, #3318, #6877, #10144, #2491, #871, #10251, #9772, #7548, #6826, #819, #1767, #42, #6041, #6936, #7603, #7714, #9427, #2713, #7769, #10311, #9317, #1710, #6098, #2543, #9483, #3425, #5196, #10198, #94, #5980, #5875, #5141, #1880, #1823, #5248, #9269, #8652, #8487, #978, #8600, #4356, #9371, #5083, #3371, #3536, #2658, #8544, #925, #4306, #4150, #1662, #8434, #6773, #5932, #10546, #7999, #3707, #1094, #2166, #6217, #1034, #6330, #2942, #9659, #6387, #1991, #4481, #7887, #9713, #3827, #2767, #2050, #3593, #6992, #1155, #5364, #265, #4535, #4652, #6154, #382, #1274, #3648, #321, #5423, #1933, #9598, #10596, #2828, #8890, #5306, #2997, #4421, #10370, #5481, #1212, #8828, #9775, #7045, #8716, #8058, #9539, #4595, #7107, #10425, #7824, #443, #8775, #7939, #10487, #2885, #6272, #7216, #3769, #7162, #2105, #5541, #207, #1382, #1489, #10034, #2320, #3883, #2417, #5650, #7326, #10718, #3153, #5701, #5758, #5598, #3101, #6449, #4089, #9100, #4865, #8944, #8993, #1336, #9046, #9881, #9988, #6659, #652, #9152, #4705, #7275, #2372, #8269, #4031, #8111, #4758, #2219, #4916, #10660, #7436, #3989, #8166, #496, #1538, #2268, #556, #3051, #3934, #6553, #8315, #9828, #6499, #1437, #10816, #9936, #4813, #3204, #8220, #6607, #608, #7382, #10762, #708, #7486, #10869, #3258, #2644, #2479, #4187, #3308, #969, #2583, #10187, #5808, #5866, #9206, #5922, #6760, #6865, #3526, #8533, #6031, #1592, #9415, #8590, #10971, #3360, #4345, #809, #7757, #5074, #10238, #8475, #9357, #7647, #4142, #3414, #136, #7703, #6926, #4972, #10298, #10133, #1809, #5181, #8373, #1700, #2533, #5026, #82, #912, #9308, #5969, #1754, #3468, #31, #7539, #760, #10918, #4294, #5128, #860, #9258, #6705, #4242, #10082, #1651, #8426, #6817, #7589, #3638, #2757, #9528, #1200, #5468, #4407, #3694, #5238, #8642, #2814, #7035, #1921, #6201, #6319, #7816, #9650, #2934, #6142, #1980, #309, #3580, #7875, #1264, #4469, #10535, #6982, #4643, #6086, #1022, #9473, #2039, #8706, #195, #10413, #5413, #5295, #1867, #5350, #10360, #7096, #9588, #4580, #8877, #1081, #6263, #7988, #8045, #254, #10474, #8817, #373, #8764, #1144, #7153, #582, #9703, #3756, #7929, #2095, #3967, #7356, #2874, #2700, #4526, #10941, #4947, #6527, #784, #733, #6734, #7464, #9177, #633, #1677, #4890, #8292, #679, #9964, #1619, #2446, #7408, #7564, #4116, #4012, #833, #4841, #10057, #10842, #2297, #5838, #5783, #2345, #9236, #3286, #3330, #10790, #5734, #9910, #4214, #4163, #8350, #5683, #3179, #4062, #6585, #5049, #4998, #8449, #10108, #3227, #9128, #2505, #6634, #2393, #10011, #1515, #10744, #8400, #9076, #3131, #7513, #6681, #10896 ),
 ( #1564, #1467, #5894, #8249, #9285, #6112, #5211, #1950, #8561, #7676, #3441, #9497, #10385, #9332, #8615, #10161, #2559, #7730, #941, #6839, #109, #225, #10210, #1893, #10329, #4266, #4438, #993, #887, #8730, #1724, #6949, #4321, #5945, #2729, #2675, #2610, #5263, #167, #3610, #8504, #5998, #6791, #1115, #8669, #1840, #5099, #58, #3493, #9387, #9557, #1050, #5319, #7007, #6896, #1782, #7839, #10267, #6055, #9443, #5154, #7619, #2781, #4373, #4, #7785, #3552, #6169, #3384, #4495, #6232, #10442, #1229, #5498, #10611, #2064, #9673, #7176, #2121, #278, #8958, #8074, #2845, #2177, #3663, #8902, #456, #3010, #2009, #4610, #2901, #8014, #5382, #7059, #1169, #1289, #5437, #9613, #8842, #9788, #398, #8788, #4548, #4667, #3725, #7954, #3786, #3840, #336, #7122, #10559, #10502, #2956, #6341, #7231, #5560, #6288, #9727, #6402, #1349, #4717, #8124, #7900, #1930, #920, #9479, #7883, #6213, #262, #5303, #8650, #8714, #9595, #10367, #4418, #2762, #2708, #3645, #1031, #10195, #4478, #7822, #10420, #147, #1875, #4303, #5360, #8597, #976, #4354, #6150, #6095, #3477, #4532, #7765, #3422, #1089, #7041, #203, #8772, #3532, #6874, #10247, #2823, #1988, #5137, #3589, #5977, #9367, #6934, #10307, #2656, #5245, #1151, #8541, #9535, #7937, #6038, #6989, #6824, #7711, #2593, #1764, #5191, #92, #9422, #1820, #3702, #6270, #4754, #493, #4703, #9043, #7159, #4589, #7321, #9656, #8109, #6381, #7995, #7104, #552, #1270, #379, #2881, #2940, #5536, #10713, #2048, #5419, #3765, #3879, #8941, #10542, #7270, #1435, #10655, #8824, #4809, #8055, #9710, #2102, #1333, #3048, #8162, #6327, #5476, #1209, #6496, #6442, #9825, #315, #8884, #10484, #440, #4648, #1379, #3825, #2216, #3931, #7213, #3099, #9878, #10593, #2993, #2264, #9770, #5647, #2161, #5595, #8989, #755, #10031, #6547, #5804, #6756, #10077, #10128, #3986, #2528, #1534, #5023, #9255, #1645, #4086, #2369, #7431, #2474, #3306, #8311, #4969, #8369, #5861, #2413, #9932, #4182, #2317, #6701, #4028, #605, #10864, #4863, #9202, #4913, #8422, #10965, #649, #4139, #806, #5917, #10810, #1586, #7586, #3354, #5699, #3255, #9304, #1696, #8214, #7379, #7536, #10758, #3150, #10914, #9094, #1487, #7483, #8266, #3201, #6604, #9983, #5755, #9148, #704, #6654, #8921, #3627, #3806, #5338, #8805, #357, #421, #241, #1968, #1069, #9747, #3744, #7974, #3567, #7022, #6967, #3680, #4513, #4629, #1310, #6307, #7196, #10347, #10577, #6359, #8750, #1131, #2142, #9574, #5517, #2862, #8031, #6249, #7141, #5399, #1910, #1187, #4685, #5455, #8092, #2744, #6131, #7916, #2973, #9514, #5281, #10460, #296, #2800, #8862, #9689, #7080, #10521, #2920, #1249, #4566, #8690, #4457, #7859, #2082, #10401, #9634, #6188, #2027, #5627, #475, #5736, #9965, #9078, #5786 ) ),
 .UNSPECIFIED., .F., .F., .F. ) 
 B_SPLINE_SURFACE_WITH_KNOTS ( ( 2, 2 ),
 ( 3, 2, 2, 2, 2, 2, 2, 2, 2, 2, 2, 2, 2, 2, 2, 2, 2, 2, 2, 2, 2, 2, 2, 2, 2, 2, 2, 2, 2, 2, 2, 2, 2, 2, 2, 2, 2, 2, 2, 2, 2, 2, 2, 2, 2, 2, 2, 2, 2, 2, 2, 2, 2, 2, 2, 2, 2, 2, 2, 2, 2, 2, 2, 2, 2, 2, 2, 2, 2, 2, 2, 2, 2, 2, 2, 2, 2, 2, 2, 2, 2, 2, 2, 2, 2, 2, 2, 2, 2, 2, 2, 2, 2, 2, 2, 2, 2, 2, 2, 2, 2, 2, 2, 2, 2, 2, 2, 2, 2, 2, 2, 2, 2, 2, 2, 2, 2, 2, 2, 2, 2, 2, 2, 2, 2, 2, 2, 2, 2, 2, 2, 2, 2, 2, 2, 2, 2, 2, 2, 2, 2, 2, 2, 2, 2, 2, 2, 2, 2, 2, 2, 2, 2, 2, 2, 2, 2, 2, 2, 2, 2, 2, 2, 2, 2, 2, 2, 2, 2, 2, 2, 2, 2, 2, 2, 2, 2, 2, 2, 2, 2, 2, 2, 2, 2, 2, 2, 2, 2, 2, 2, 2, 3 ),
 ( 0.000000000000000000, 1.000000000000000000 ),
 ( 0.000000000000000000, 0.005208333333333333044, 0.01041666666666666609, 0.01562500000000000000, 0.02083333333333333218, 0.02604166666666666782, 0.03125000000000000000, 0.03645833333333333565, 0.04166666666666666435, 0.04687500000000000000, 0.05208333333333333565, 0.05729166666666666435, 0.06250000000000000000, 0.06770833333333332871, 0.07291666666666667129, 0.07812500000000000000, 0.08333333333333332871, 0.08854166666666667129, 0.09375000000000000000, 0.09895833333333332871, 0.1041666666666666713, 0.1093750000000000000, 0.1145833333333333287, 0.1197916666666666713, 0.1250000000000000000, 0.1302083333333333426, 0.1354166666666666574, 0.1406250000000000000, 0.1458333333333333426, 0.1510416666666666574, 0.1562500000000000000, 0.1614583333333333426, 0.1666666666666666574, 0.1718750000000000000, 0.1770833333333333426, 0.1822916666666666574, 0.1875000000000000000, 0.1927083333333333426, 0.1979166666666666574, 0.2031250000000000000, 0.2083333333333333426, 0.2135416666666666574, 0.2187500000000000000, 0.2239583333333333426, 0.2291666666666666574, 0.2343750000000000000, 0.2395833333333333426, 0.2447916666666666574, 0.2500000000000000000, 0.2552083333333333148, 0.2604166666666666852, 0.2656250000000000000, 0.2708333333333333148, 0.2760416666666666852, 0.2812500000000000000, 0.2864583333333333148, 0.2916666666666666852, 0.2968750000000000000, 0.3020833333333333148, 0.3072916666666666852, 0.3125000000000000000, 0.3177083333333333148, 0.3229166666666666852, 0.3281250000000000000, 0.3333333333333333148, 0.3385416666666666852, 0.3437500000000000000, 0.3489583333333333148, 0.3541666666666666852, 0.3593750000000000000, 0.3645833333333333148, 0.3697916666666666852, 0.3750000000000000000, 0.3802083333333333148, 0.3854166666666666852, 0.3906250000000000000, 0.3958333333333333148, 0.4010416666666666852, 0.4062500000000000000, 0.4114583333333333148, 0.4166666666666666852, 0.4218750000000000000, 0.4270833333333333148, 0.4322916666666666852, 0.4375000000000000000, 0.4427083333333333148, 0.4479166666666666852, 0.4531250000000000000, 0.4583333333333333148, 0.4635416666666666852, 0.4687500000000000000, 0.4739583333333333148, 0.4791666666666666852, 0.4843750000000000000, 0.4895833333333333148, 0.4947916666666666852, 0.5000000000000000000, 0.5052083333333333703, 0.5104166666666666297, 0.5156250000000000000, 0.5208333333333333703, 0.5260416666666666297, 0.5312500000000000000, 0.5364583333333333703, 0.5416666666666666297, 0.5468750000000000000, 0.5520833333333333703, 0.5572916666666666297, 0.5625000000000000000, 0.5677083333333333703, 0.5729166666666666297, 0.5781250000000000000, 0.5833333333333333703, 0.5885416666666666297, 0.5937500000000000000, 0.5989583333333333703, 0.6041666666666666297, 0.6093750000000000000, 0.6145833333333333703, 0.6197916666666666297, 0.6250000000000000000, 0.6302083333333333703, 0.6354166666666666297, 0.6406250000000000000, 0.6458333333333333703, 0.6510416666666666297, 0.6562500000000000000, 0.6614583333333333703, 0.6666666666666666297, 0.6718750000000000000, 0.6770833333333333703, 0.6822916666666666297, 0.6875000000000000000, 0.6927083333333333703, 0.6979166666666666297, 0.7031250000000000000, 0.7083333333333333703, 0.7135416666666666297, 0.7187500000000000000, 0.7239583333333333703, 0.7291666666666666297, 0.7343750000000000000, 0.7395833333333333703, 0.7447916666666666297, 0.7500000000000000000, 0.7552083333333333703, 0.7604166666666666297, 0.7656250000000000000, 0.7708333333333333703, 0.7760416666666666297, 0.7812500000000000000, 0.7864583333333333703, 0.7916666666666666297, 0.7968750000000000000, 0.8020833333333333703, 0.8072916666666666297, 0.8125000000000000000, 0.8177083333333333703, 0.8229166666666666297, 0.8281250000000000000, 0.8333333333333333703, 0.8385416666666666297, 0.8437500000000000000, 0.8489583333333333703, 0.8541666666666666297, 0.8593750000000000000, 0.8645833333333333703, 0.8697916666666666297, 0.8750000000000000000, 0.8802083333333333703, 0.8854166666666666297, 0.8906250000000000000, 0.8958333333333333703, 0.9010416666666666297, 0.9062500000000000000, 0.9114583333333333703, 0.9166666666666666297, 0.9218750000000000000, 0.9270833333333333703, 0.9322916666666666297, 0.9375000000000000000, 0.9427083333333333703, 0.9479166666666666297, 0.9531250000000000000, 0.9583333333333333703, 0.9635416666666666297, 0.9687500000000000000, 0.9739583333333333703, 0.9791666666666666297, 0.9843750000000000000, 0.9895833333333333703, 0.9947916666666666297, 1.000000000000000000 ),
 .UNSPECIFIED. ) 
 GEOMETRIC_REPRESENTATION_ITEM ( )  RATIONAL_B_SPLINE_SURFACE ( (
 ( 1.000000000000000000, 0.8660254037844387076, 1.000000000000000000, 0.8660254037844387076, 1.000000000000000000, 0.8660254037844387076, 1.000000000000000000, 0.8660254037844387076, 1.000000000000000000, 0.8660254037844387076, 1.000000000000000000, 0.8660254037844387076, 1.000000000000000000, 0.8660254037844387076, 1.000000000000000000, 0.8660254037844387076, 1.000000000000000000, 0.8660254037844387076, 1.000000000000000000, 0.8660254037844387076, 1.000000000000000000, 0.8660254037844387076, 1.000000000000000000, 0.8660254037844387076, 1.000000000000000000, 0.8660254037844387076, 1.000000000000000000, 0.8660254037844387076, 1.000000000000000000, 0.8660254037844387076, 1.000000000000000000, 0.8660254037844387076, 1.000000000000000000, 0.8660254037844387076, 1.000000000000000000, 0.8660254037844387076, 1.000000000000000000, 0.8660254037844387076, 1.000000000000000000, 0.8660254037844387076, 1.000000000000000000, 0.8660254037844387076, 1.000000000000000000, 0.8660254037844387076, 1.000000000000000000, 0.8660254037844387076, 1.000000000000000000, 0.8660254037844387076, 1.000000000000000000, 0.8660254037844387076, 1.000000000000000000, 0.8660254037844387076, 1.000000000000000000, 0.8660254037844387076, 1.000000000000000000, 0.8660254037844387076, 1.000000000000000000, 0.8660254037844387076, 1.000000000000000000, 0.8660254037844387076, 1.000000000000000000, 0.8660254037844387076, 1.000000000000000000, 0.8660254037844387076, 1.000000000000000000, 0.8660254037844387076, 1.000000000000000000, 0.8660254037844387076, 1.000000000000000000, 0.8660254037844387076, 1.000000000000000000, 0.8660254037844387076, 1.000000000000000000, 0.8660254037844387076, 1.000000000000000000, 0.8660254037844387076, 1.000000000000000000, 0.8660254037844387076, 1.000000000000000000, 0.8660254037844387076, 1.000000000000000000, 0.8660254037844387076, 1.000000000000000000, 0.8660254037844387076, 1.000000000000000000, 0.8660254037844387076, 1.000000000000000000, 0.8660254037844387076, 1.000000000000000000, 0.8660254037844387076, 1.000000000000000000, 0.8660254037844387076, 1.000000000000000000, 0.8660254037844387076, 1.000000000000000000, 0.8660254037844387076, 1.000000000000000000, 0.8660254037844387076, 1.000000000000000000, 0.8660254037844387076, 1.000000000000000000, 0.8660254037844387076, 1.000000000000000000, 0.8660254037844387076, 1.000000000000000000, 0.8660254037844387076, 1.000000000000000000, 0.8660254037844387076, 1.000000000000000000, 0.8660254037844387076, 1.000000000000000000, 0.8660254037844387076, 1.000000000000000000, 0.8660254037844387076, 1.000000000000000000, 0.8660254037844387076, 1.000000000000000000, 0.8660254037844387076, 1.000000000000000000, 0.8660254037844387076, 1.000000000000000000, 0.8660254037844387076, 1.000000000000000000, 0.8660254037844387076, 1.000000000000000000, 0.8660254037844387076, 1.000000000000000000, 0.8660254037844387076, 1.000000000000000000, 0.8660254037844387076, 1.000000000000000000, 0.8660254037844387076, 1.000000000000000000, 0.8660254037844387076, 1.000000000000000000, 0.8660254037844387076, 1.000000000000000000, 0.8660254037844387076, 1.000000000000000000, 0.8660254037844387076, 1.000000000000000000, 0.8660254037844387076, 1.000000000000000000, 0.8660254037844387076, 1.000000000000000000, 0.8660254037844387076, 1.000000000000000000, 0.8660254037844387076, 1.000000000000000000, 0.8660254037844387076, 1.000000000000000000, 0.8660254037844387076, 1.000000000000000000, 0.8660254037844387076, 1.000000000000000000, 0.8660254037844387076, 1.000000000000000000, 0.8660254037844387076, 1.000000000000000000, 0.8660254037844387076, 1.000000000000000000, 0.8660254037844387076, 1.000000000000000000, 0.8660254037844387076, 1.000000000000000000, 0.8660254037844387076, 1.000000000000000000, 0.8660254037844387076, 1.000000000000000000, 0.8660254037844387076, 1.000000000000000000, 0.8660254037844387076, 1.000000000000000000, 0.8660254037844387076, 1.000000000000000000, 0.8660254037844387076, 1.000000000000000000, 0.8660254037844387076, 1.000000000000000000, 0.8660254037844387076, 1.000000000000000000, 0.8660254037844387076, 1.000000000000000000, 0.8660254037844387076, 1.000000000000000000, 0.8660254037844387076, 1.000000000000000000, 0.8660254037844387076, 1.000000000000000000, 0.8660254037844387076, 1.000000000000000000, 0.8660254037844387076, 1.000000000000000000, 0.8660254037844387076, 1.000000000000000000, 0.8660254037844387076, 1.000000000000000000, 0.8660254037844387076, 1.000000000000000000, 0.8660254037844387076, 1.000000000000000000, 0.8660254037844387076, 1.000000000000000000, 0.8660254037844387076, 1.000000000000000000, 0.8660254037844387076, 1.000000000000000000, 0.8660254037844387076, 1.000000000000000000, 0.8660254037844387076, 1.000000000000000000, 0.8660254037844387076, 1.000000000000000000, 0.8660254037844387076, 1.000000000000000000, 0.8660254037844387076, 1.000000000000000000, 0.8660254037844387076, 1.000000000000000000, 0.8660254037844387076, 1.000000000000000000, 0.8660254037844387076, 1.000000000000000000, 0.8660254037844387076, 1.000000000000000000, 0.8660254037844387076, 1.000000000000000000, 0.8660254037844387076, 1.000000000000000000, 0.8660254037844387076, 1.000000000000000000, 0.8660254037844387076, 1.000000000000000000, 0.8660254037844387076, 1.000000000000000000, 0.8660254037844387076, 1.000000000000000000, 0.8660254037844387076, 1.000000000000000000, 0.8660254037844387076, 1.000000000000000000, 0.8660254037844387076, 1.000000000000000000, 0.8660254037844387076, 1.000000000000000000, 0.8660254037844387076, 1.000000000000000000, 0.8660254037844387076, 1.000000000000000000, 0.8660254037844387076, 1.000000000000000000, 0.8660254037844387076, 1.000000000000000000, 0.8660254037844387076, 1.000000000000000000, 0.8660254037844387076, 1.000000000000000000, 0.8660254037844387076, 1.000000000000000000, 0.8660254037844387076, 1.000000000000000000, 0.8660254037844387076, 1.000000000000000000, 0.8660254037844387076, 1.000000000000000000, 0.8660254037844387076, 1.000000000000000000, 0.8660254037844387076, 1.000000000000000000, 0.8660254037844387076, 1.000000000000000000, 0.8660254037844387076, 1.000000000000000000, 0.8660254037844387076, 1.000000000000000000, 0.8660254037844387076, 1.000000000000000000, 0.8660254037844387076, 1.000000000000000000, 0.8660254037844387076, 1.000000000000000000, 0.8660254037844387076, 1.000000000000000000, 0.8660254037844387076, 1.000000000000000000, 0.8660254037844387076, 1.000000000000000000, 0.8660254037844387076, 1.000000000000000000, 0.8660254037844387076, 1.000000000000000000, 0.8660254037844387076, 1.000000000000000000, 0.8660254037844387076, 1.000000000000000000, 0.8660254037844387076, 1.000000000000000000, 0.8660254037844387076, 1.000000000000000000, 0.8660254037844387076, 1.000000000000000000, 0.8660254037844387076, 1.000000000000000000, 0.8660254037844387076, 1.000000000000000000, 0.8660254037844387076, 1.000000000000000000, 0.8660254037844387076, 1.000000000000000000, 0.8660254037844387076, 1.000000000000000000, 0.8660254037844387076, 1.000000000000000000, 0.8660254037844387076, 1.000000000000000000, 0.8660254037844387076, 1.000000000000000000, 0.8660254037844387076, 1.000000000000000000, 0.8660254037844387076, 1.000000000000000000, 0.8660254037844387076, 1.000000000000000000, 0.8660254037844387076, 1.000000000000000000, 0.8660254037844387076, 1.000000000000000000, 0.8660254037844387076, 1.000000000000000000, 0.8660254037844387076, 1.000000000000000000, 0.8660254037844387076, 1.000000000000000000, 0.8660254037844387076, 1.000000000000000000, 0.8660254037844387076, 1.000000000000000000, 0.8660254037844387076, 1.000000000000000000, 0.8660254037844387076, 1.000000000000000000, 0.8660254037844387076, 1.000000000000000000, 0.8660254037844387076, 1.000000000000000000, 0.8660254037844387076, 1.000000000000000000, 0.8660254037844387076, 1.000000000000000000, 0.8660254037844387076, 1.000000000000000000, 0.8660254037844387076, 1.000000000000000000, 0.8660254037844387076, 1.000000000000000000, 0.8660254037844387076, 1.000000000000000000, 0.8660254037844387076, 1.000000000000000000, 0.8660254037844387076, 1.000000000000000000, 0.8660254037844387076, 1.000000000000000000, 0.8660254037844387076, 1.000000000000000000, 0.8660254037844387076, 1.000000000000000000, 0.8660254037844387076, 1.000000000000000000, 0.8660254037844387076, 1.000000000000000000, 0.8660254037844387076, 1.000000000000000000, 0.8660254037844387076, 1.000000000000000000, 0.8660254037844387076, 1.000000000000000000, 0.8660254037844387076, 1.000000000000000000, 0.8660254037844387076, 1.000000000000000000, 0.8660254037844387076, 1.000000000000000000, 0.8660254037844387076, 1.000000000000000000),
 ( 1.000000000000000000, 0.8660254037844387076, 1.000000000000000000, 0.8660254037844387076, 1.000000000000000000, 0.8660254037844387076, 1.000000000000000000, 0.8660254037844387076, 1.000000000000000000, 0.8660254037844387076, 1.000000000000000000, 0.8660254037844387076, 1.000000000000000000, 0.8660254037844387076, 1.000000000000000000, 0.8660254037844387076, 1.000000000000000000, 0.8660254037844387076, 1.000000000000000000, 0.8660254037844387076, 1.000000000000000000, 0.8660254037844387076, 1.000000000000000000, 0.8660254037844387076, 1.000000000000000000, 0.8660254037844387076, 1.000000000000000000, 0.8660254037844387076, 1.000000000000000000, 0.8660254037844387076, 1.000000000000000000, 0.8660254037844387076, 1.000000000000000000, 0.8660254037844387076, 1.000000000000000000, 0.8660254037844387076, 1.000000000000000000, 0.8660254037844387076, 1.000000000000000000, 0.8660254037844387076, 1.000000000000000000, 0.8660254037844387076, 1.000000000000000000, 0.8660254037844387076, 1.000000000000000000, 0.8660254037844387076, 1.000000000000000000, 0.8660254037844387076, 1.000000000000000000, 0.8660254037844387076, 1.000000000000000000, 0.8660254037844387076, 1.000000000000000000, 0.8660254037844387076, 1.000000000000000000, 0.8660254037844387076, 1.000000000000000000, 0.8660254037844387076, 1.000000000000000000, 0.8660254037844387076, 1.000000000000000000, 0.8660254037844387076, 1.000000000000000000, 0.8660254037844387076, 1.000000000000000000, 0.8660254037844387076, 1.000000000000000000, 0.8660254037844387076, 1.000000000000000000, 0.8660254037844387076, 1.000000000000000000, 0.8660254037844387076, 1.000000000000000000, 0.8660254037844387076, 1.000000000000000000, 0.8660254037844387076, 1.000000000000000000, 0.8660254037844387076, 1.000000000000000000, 0.8660254037844387076, 1.000000000000000000, 0.8660254037844387076, 1.000000000000000000, 0.8660254037844387076, 1.000000000000000000, 0.8660254037844387076, 1.000000000000000000, 0.8660254037844387076, 1.000000000000000000, 0.8660254037844387076, 1.000000000000000000, 0.8660254037844387076, 1.000000000000000000, 0.8660254037844387076, 1.000000000000000000, 0.8660254037844387076, 1.000000000000000000, 0.8660254037844387076, 1.000000000000000000, 0.8660254037844387076, 1.000000000000000000, 0.8660254037844387076, 1.000000000000000000, 0.8660254037844387076, 1.000000000000000000, 0.8660254037844387076, 1.000000000000000000, 0.8660254037844387076, 1.000000000000000000, 0.8660254037844387076, 1.000000000000000000, 0.8660254037844387076, 1.000000000000000000, 0.8660254037844387076, 1.000000000000000000, 0.8660254037844387076, 1.000000000000000000, 0.8660254037844387076, 1.000000000000000000, 0.8660254037844387076, 1.000000000000000000, 0.8660254037844387076, 1.000000000000000000, 0.8660254037844387076, 1.000000000000000000, 0.8660254037844387076, 1.000000000000000000, 0.8660254037844387076, 1.000000000000000000, 0.8660254037844387076, 1.000000000000000000, 0.8660254037844387076, 1.000000000000000000, 0.8660254037844387076, 1.000000000000000000, 0.8660254037844387076, 1.000000000000000000, 0.8660254037844387076, 1.000000000000000000, 0.8660254037844387076, 1.000000000000000000, 0.8660254037844387076, 1.000000000000000000, 0.8660254037844387076, 1.000000000000000000, 0.8660254037844387076, 1.000000000000000000, 0.8660254037844387076, 1.000000000000000000, 0.8660254037844387076, 1.000000000000000000, 0.8660254037844387076, 1.000000000000000000, 0.8660254037844387076, 1.000000000000000000, 0.8660254037844387076, 1.000000000000000000, 0.8660254037844387076, 1.000000000000000000, 0.8660254037844387076, 1.000000000000000000, 0.8660254037844387076, 1.000000000000000000, 0.8660254037844387076, 1.000000000000000000, 0.8660254037844387076, 1.000000000000000000, 0.8660254037844387076, 1.000000000000000000, 0.8660254037844387076, 1.000000000000000000, 0.8660254037844387076, 1.000000000000000000, 0.8660254037844387076, 1.000000000000000000, 0.8660254037844387076, 1.000000000000000000, 0.8660254037844387076, 1.000000000000000000, 0.8660254037844387076, 1.000000000000000000, 0.8660254037844387076, 1.000000000000000000, 0.8660254037844387076, 1.000000000000000000, 0.8660254037844387076, 1.000000000000000000, 0.8660254037844387076, 1.000000000000000000, 0.8660254037844387076, 1.000000000000000000, 0.8660254037844387076, 1.000000000000000000, 0.8660254037844387076, 1.000000000000000000, 0.8660254037844387076, 1.000000000000000000, 0.8660254037844387076, 1.000000000000000000, 0.8660254037844387076, 1.000000000000000000, 0.8660254037844387076, 1.000000000000000000, 0.8660254037844387076, 1.000000000000000000, 0.8660254037844387076, 1.000000000000000000, 0.8660254037844387076, 1.000000000000000000, 0.8660254037844387076, 1.000000000000000000, 0.8660254037844387076, 1.000000000000000000, 0.8660254037844387076, 1.000000000000000000, 0.8660254037844387076, 1.000000000000000000, 0.8660254037844387076, 1.000000000000000000, 0.8660254037844387076, 1.000000000000000000, 0.8660254037844387076, 1.000000000000000000, 0.8660254037844387076, 1.000000000000000000, 0.8660254037844387076, 1.000000000000000000, 0.8660254037844387076, 1.000000000000000000, 0.8660254037844387076, 1.000000000000000000, 0.8660254037844387076, 1.000000000000000000, 0.8660254037844387076, 1.000000000000000000, 0.8660254037844387076, 1.000000000000000000, 0.8660254037844387076, 1.000000000000000000, 0.8660254037844387076, 1.000000000000000000, 0.8660254037844387076, 1.000000000000000000, 0.8660254037844387076, 1.000000000000000000, 0.8660254037844387076, 1.000000000000000000, 0.8660254037844387076, 1.000000000000000000, 0.8660254037844387076, 1.000000000000000000, 0.8660254037844387076, 1.000000000000000000, 0.8660254037844387076, 1.000000000000000000, 0.8660254037844387076, 1.000000000000000000, 0.8660254037844387076, 1.000000000000000000, 0.8660254037844387076, 1.000000000000000000, 0.8660254037844387076, 1.000000000000000000, 0.8660254037844387076, 1.000000000000000000, 0.8660254037844387076, 1.000000000000000000, 0.8660254037844387076, 1.000000000000000000, 0.8660254037844387076, 1.000000000000000000, 0.8660254037844387076, 1.000000000000000000, 0.8660254037844387076, 1.000000000000000000, 0.8660254037844387076, 1.000000000000000000, 0.8660254037844387076, 1.000000000000000000, 0.8660254037844387076, 1.000000000000000000, 0.8660254037844387076, 1.000000000000000000, 0.8660254037844387076, 1.000000000000000000, 0.8660254037844387076, 1.000000000000000000, 0.8660254037844387076, 1.000000000000000000, 0.8660254037844387076, 1.000000000000000000, 0.8660254037844387076, 1.000000000000000000, 0.8660254037844387076, 1.000000000000000000, 0.8660254037844387076, 1.000000000000000000, 0.8660254037844387076, 1.000000000000000000, 0.8660254037844387076, 1.000000000000000000, 0.8660254037844387076, 1.000000000000000000, 0.8660254037844387076, 1.000000000000000000, 0.8660254037844387076, 1.000000000000000000, 0.8660254037844387076, 1.000000000000000000, 0.8660254037844387076, 1.000000000000000000, 0.8660254037844387076, 1.000000000000000000, 0.8660254037844387076, 1.000000000000000000, 0.8660254037844387076, 1.000000000000000000, 0.8660254037844387076, 1.000000000000000000, 0.8660254037844387076, 1.000000000000000000, 0.8660254037844387076, 1.000000000000000000, 0.8660254037844387076, 1.000000000000000000, 0.8660254037844387076, 1.000000000000000000, 0.8660254037844387076, 1.000000000000000000, 0.8660254037844387076, 1.000000000000000000, 0.8660254037844387076, 1.000000000000000000, 0.8660254037844387076, 1.000000000000000000, 0.8660254037844387076, 1.000000000000000000, 0.8660254037844387076, 1.000000000000000000, 0.8660254037844387076, 1.000000000000000000, 0.8660254037844387076, 1.000000000000000000, 0.8660254037844387076, 1.000000000000000000, 0.8660254037844387076, 1.000000000000000000, 0.8660254037844387076, 1.000000000000000000, 0.8660254037844387076, 1.000000000000000000, 0.8660254037844387076, 1.000000000000000000, 0.8660254037844387076, 1.000000000000000000, 0.8660254037844387076, 1.000000000000000000, 0.8660254037844387076, 1.000000000000000000, 0.8660254037844387076, 1.000000000000000000, 0.8660254037844387076, 1.000000000000000000, 0.8660254037844387076, 1.000000000000000000, 0.8660254037844387076, 1.000000000000000000, 0.8660254037844387076, 1.000000000000000000, 0.8660254037844387076, 1.000000000000000000, 0.8660254037844387076, 1.000000000000000000, 0.8660254037844387076, 1.000000000000000000, 0.8660254037844387076, 1.000000000000000000, 0.8660254037844387076, 1.000000000000000000, 0.8660254037844387076, 1.000000000000000000, 0.8660254037844387076, 1.000000000000000000, 0.8660254037844387076, 1.000000000000000000) ) ) 
 REPRESENTATION_ITEM ( '' )  SURFACE ( )  );
#2892 = LINE ( 'NONE', #1885, #358 ) ;
#2893 = CIRCLE ( 'NONE', #3776, 1.000000000000000888 ) ;
#2894 = ORIENTED_EDGE ( 'NONE', *, *, #10862, .F. ) ;
#2895 = CARTESIAN_POINT ( 'NONE',  ( -61.13531646874998415, 16.07812499965860198, 1.500000000000002220 ) ) ;
#2896 = CARTESIAN_POINT ( 'NONE',  ( -62.49999999999998579, 9.635416665983870033, 2.366025403784441483 ) ) ;
#2897 = FACE_OUTER_BOUND ( 'NONE', #3419, .T. ) ;
#2898 = LINE ( 'NONE', #10610, #7430 ) ;
#2899 = CIRCLE ( 'NONE', #9104, 1.000000000000000888 ) ;
#2900 = CARTESIAN_POINT ( 'NONE',  ( -61.99999999999999289, 14.82812499965860020, 2.498450539062049724 ) ) ;
#2901 = CARTESIAN_POINT ( 'NONE',  ( -62.86468353124999453, 9.953124999658601979, 1.500000000000002220 ) ) ;
#2902 = EDGE_CURVE ( 'NONE', #3086, #4883, #1753, .T. ) ;
#2903 = CARTESIAN_POINT ( 'NONE',  ( -62.49999999999998579, 11.38541666598387003, 2.366025403784441483 ) ) ;
#2904 = PLANE ( 'NONE',  #9212 ) ;
#2905 = CARTESIAN_POINT ( 'NONE',  ( -62.86468353124999453, 10.76562499965860020, 1.500000000000002220 ) ) ;
#2906 = DIRECTION ( 'NONE',  ( 0.000000000000000000, 0.000000000000000000, -1.000000000000000000 ) ) ;
#2907 = ORIENTED_EDGE ( 'NONE', *, *, #9894, .T. ) ;
#2908 = CARTESIAN_POINT ( 'NONE',  ( -61.73205080756886076, 13.91741454900183150, 2.500000000000003109 ) ) ;
#2909 = LINE ( 'NONE', #6296, #234 ) ;
#2910 = EDGE_LOOP ( 'NONE', ( #3732, #5460, #8389, #1222 ) ) ;
#2911 = CARTESIAN_POINT ( 'NONE',  ( -62.49999999999998579, 10.30208333265053611, 0.6339745962155627357 ) ) ;
#2912 = CARTESIAN_POINT ( 'NONE',  ( -61.13531646874998415, 12.32812499965860198, 1.500000000000002220 ) ) ;
#2913 = CARTESIAN_POINT ( 'NONE',  ( -61.56765823437498142, 10.11979166632526805, 0.7511620957034663704 ) ) ;
#2914 = DIRECTION ( 'NONE',  ( 0.000000000000000000, 1.000000000000000000, 0.000000000000000000 ) ) ;
#2915 = ORIENTED_EDGE ( 'NONE', *, *, #4504, .T. ) ;
#2916 = LINE ( 'NONE', #6304, #5810 ) ;
#2917 = CARTESIAN_POINT ( 'NONE',  ( -62.86468353124999453, 10.26562499965860198, 1.500000000000002220 ) ) ;
#2918 = EDGE_CURVE ( 'NONE', #6183, #2234, #6759, .T. ) ;
#2919 = APPLICATION_PROTOCOL_DEFINITION ( 'draft international standard', 'automotive_design', 1998, #10669 ) ;
#2920 = CARTESIAN_POINT ( 'NONE',  ( -62.43234176562499016, 15.74479166632526628, 2.248837904296538071 ) ) ;
#2921 = VECTOR ( 'NONE', #8474, 1000.000000000000000 ) ;
#2922 = CARTESIAN_POINT ( 'NONE',  ( -61.49999999999998579, 15.17708333265053611, 2.366025403784441927 ) ) ;
#2923 = DIRECTION ( 'NONE',  ( -0.000000000000000000, -1.000000000000000000, -0.000000000000000000 ) ) ;
#2924 = ORIENTED_EDGE ( 'NONE', *, *, #2766, .F. ) ;
#2925 = EDGE_CURVE ( 'NONE', #9418, #5688, #808, .T. ) ;
#2926 = CARTESIAN_POINT ( 'NONE',  ( -61.49999999999998579, 15.26041666598387003, 0.6339745962155628467 ) ) ;
#2927 = ORIENTED_EDGE ( 'NONE', *, *, #1789, .F. ) ;
#2928 = CARTESIAN_POINT ( 'NONE',  ( -61.56765823437498852, 13.03645833299193413, 2.248837904296538515 ) ) ;
#2929 = FACE_OUTER_BOUND ( 'NONE', #9248, .T. ) ;
#2930 = LINE ( 'NONE', #9699, #3413 ) ;
#2931 = ORIENTED_EDGE ( 'NONE', *, *, #6699, .T. ) ;
#2932 = CARTESIAN_POINT ( 'NONE',  ( -60.99999999999998579, 12.22916666666666607, 2.077350269189628840 ) ) ;
#2933 = CARTESIAN_POINT ( 'NONE',  ( -61.99999999999998579, 10.18750000000000000, 2.500000000000002665 ) ) ;
#2934 = CARTESIAN_POINT ( 'NONE',  ( -61.56765823437498142, 13.93229166632526805, 0.7511620957034663704 ) ) ;
#2935 = DIRECTION ( 'NONE',  ( -0.000000000000000000, -1.000000000000000000, -0.000000000000000000 ) ) ;
#2936 = CARTESIAN_POINT ( 'NONE',  ( -60.99999999999998579, 10.69791666598386826, 2.077350269189628840 ) ) ;
#2937 = VERTEX_POINT ( 'NONE', #8232 ) ;
#2938 = CARTESIAN_POINT ( 'NONE',  ( -61.99999999999998579, 9.031249999317202182, 0.5000000000000013323 ) ) ;
#2939 = DIRECTION ( 'NONE',  ( 1.000000000000000000, 0.000000000000000000, -0.000000000000000000 ) ) ;
#2940 = CARTESIAN_POINT ( 'NONE',  ( -61.13531646874998415, 12.34895833299193413, 1.000774730468978468 ) ) ;
#2941 = VERTEX_POINT ( 'NONE', #1808 ) ;
#2942 = CARTESIAN_POINT ( 'NONE',  ( -62.86468353124999453, 9.765624999658601979, 1.500000000000002220 ) ) ;
#2943 = DIRECTION ( 'NONE',  ( 0.000000000000000000, 1.000000000000000000, 0.000000000000000000 ) ) ;
#2944 = CARTESIAN_POINT ( 'NONE',  ( -61.13531646874998415, 14.89062499965860020, 1.500000000000002220 ) ) ;
#2945 = DIRECTION ( 'NONE',  ( -0.000000000000000000, -1.000000000000000000, -0.000000000000000000 ) ) ;
#2946 = ORIENTED_EDGE ( 'NONE', *, *, #9058, .F. ) ;
#2947 = ADVANCED_FACE ( 'NONE', ( #5921 ), #9307, .F. ) ;
#2948 = CARTESIAN_POINT ( 'NONE',  ( -60.99999999999998579, 10.50000000000000000, 1.500000000000002220 ) ) ;
#2949 = EDGE_LOOP ( 'NONE', ( #9711, #5951, #8530, #9448, #4313, #264, #9290, #9116, #7777, #10190, #6222, #9896, #9511, #2704, #4881, #245, #6159, #5797, #5538, #10580, #10595, #2074, #2078, #6081, #80, #9141, #5924, #5134, #9365, #1884, #3601, #7168, #6310, #1099, #10456, #1964, #2104, #4176, #8340, #8102, #748, #10526, #2772, #10101, #1305, #9150, #1971, #3834, #8363, #7644, #6940, #2370, #3390, #2603, #10154, #5055, #8593, #2871, #8588, #8429, #10090, #7862, #5333, #2867, #4189, #10423, #5514, #8080, #9278 ) ) ;
#2950 = CARTESIAN_POINT ( 'NONE',  ( -61.99999999999998579, 11.81250000000000000, 0.5000000000000013323 ) ) ;
#2951 = EDGE_CURVE ( 'NONE', #10259, #6433, #2582, .T. ) ;
#2952 = CARTESIAN_POINT ( 'NONE',  ( -61.56765823437498852, 16.03645833299193768, 2.248837904296538515 ) ) ;
#2953 = CARTESIAN_POINT ( 'NONE',  ( -120.0000000000000000, -15.00000000000001421, 83.15773105863907233 ) ) ;
#2954 = CARTESIAN_POINT ( 'NONE',  ( 140.0000000000000284, 2.500000000000000000, 3.000000000000000000 ) ) ;
#2955 = CARTESIAN_POINT ( 'NONE',  ( -139.9999999999999716, -8.000000000000000000, 3.000000000000000000 ) ) ;
#2956 = CARTESIAN_POINT ( 'NONE',  ( -62.43234176562498305, 10.41145833299193413, 0.7511620957034662593 ) ) ;
#2957 = CARTESIAN_POINT ( 'NONE',  ( -60.99999999999998579, 11.98958333265053611, 0.9226497308103762673 ) ) ;
#2958 =( BOUNDED_CURVE ( )  B_SPLINE_CURVE ( 2, ( #5097, #165, #7617, #2, #8502, #6947, #10939, #885, #1675 ),
 .UNSPECIFIED., .F., .F. ) 
 B_SPLINE_CURVE_WITH_KNOTS ( ( 3, 2, 2, 2, 3 ),
 ( 0.3359374999999999445, 0.3385416666666666852, 0.3437500000000000000, 0.3489583333333333148, 0.3515625000000000000 ),
 .UNSPECIFIED. ) 
 CURVE ( )  GEOMETRIC_REPRESENTATION_ITEM ( )  RATIONAL_B_SPLINE_CURVE ( ( 0.9330127018922192983, 0.9330127018922178550, 1.000000000000000000, 0.8660254037844387076, 1.000000000000000000, 0.8660254037844387076, 1.000000000000000000, 0.9330127018922194093, 0.9330127018922194093 ) ) 
 REPRESENTATION_ITEM ( '' )  );
#2959 = DIRECTION ( 'NONE',  ( 0.000000000000000000, -1.000000000000000000, 0.000000000000000000 ) ) ;
#2960 = CARTESIAN_POINT ( 'NONE',  ( -62.43234176562498305, 9.973958332991934128, 0.7511620957034662593 ) ) ;
#2961 = CARTESIAN_POINT ( 'NONE',  ( -77.99999999999998579, 11.49999999999999645, 8.600860617226443239 ) ) ;
#2962 = ORIENTED_EDGE ( 'NONE', *, *, #8420, .F. ) ;
#2963 = LINE ( 'NONE', #2129, #1045 ) ;
#2964 = CARTESIAN_POINT ( 'NONE',  ( -61.73205080756886076, 15.30133545031537068, 0.5000000000000014433 ) ) ;
#2965 = ORIENTED_EDGE ( 'NONE', *, *, #7885, .F. ) ;
#2966 = CARTESIAN_POINT ( 'NONE',  ( -60.99999999999998579, 15.72916666666666430, 2.077350269189628840 ) ) ;
#2967 = CARTESIAN_POINT ( 'NONE',  ( -61.56765823437498142, 12.11979166632526628, 0.7511620957034663704 ) ) ;
#2968 = CARTESIAN_POINT ( 'NONE',  ( -61.13531646874997705, 10.34895833299193413, 1.000774730468978468 ) ) ;
#2969 = ORIENTED_EDGE ( 'NONE', *, *, #5488, .F. ) ;
#2970 = DIRECTION ( 'NONE',  ( -0.000000000000000000, -1.000000000000000000, -0.000000000000000000 ) ) ;
#2971 = CARTESIAN_POINT ( 'NONE',  ( -61.99999999999999289, 10.95312499965860020, 0.5015494609379544944 ) ) ;
#2972 = DIRECTION ( 'NONE',  ( 0.000000000000000000, 0.000000000000000000, 1.000000000000000000 ) ) ;
#2973 = CARTESIAN_POINT ( 'NONE',  ( -61.56765823437498852, 15.53645833299193590, 2.248837904296538515 ) ) ;
#2974 = CARTESIAN_POINT ( 'NONE',  ( -62.49999999999998579, 14.05208333265053611, 0.6339745962155627357 ) ) ;
#2975 = CARTESIAN_POINT ( 'NONE',  ( -149.9999999999999716, -8.000000000000000000, 0.000000000000000000 ) ) ;
#2976 = ORIENTED_EDGE ( 'NONE', *, *, #10172, .T. ) ;
#2977 = ADVANCED_FACE ( 'NONE', ( #6925 ), #3524, .F. ) ;
#2978 =( NAMED_UNIT ( * ) SI_UNIT ( $, .STERADIAN. ) SOLID_ANGLE_UNIT ( ) );
#2979 = VERTEX_POINT ( 'NONE', #8532 ) ;
#2980 = EDGE_CURVE ( 'NONE', #8205, #6709, #3997, .T. ) ;
#2981 = CARTESIAN_POINT ( 'NONE',  ( -61.13531646874997705, 13.34895833299193413, 1.000774730468978468 ) ) ;
#2982 = PRESENTATION_LAYER_ASSIGNMENT (  '', '', ( #4910 ) ) ;
#2983 = CARTESIAN_POINT ( 'NONE',  ( -60.99999999999998579, 11.77083333333333393, 0.9226497308103762673 ) ) ;
#2984 = ORIENTED_EDGE ( 'NONE', *, *, #7638, .T. ) ;
#2985 = CARTESIAN_POINT ( 'NONE',  ( -61.49999999999998579, 12.95833333333333215, 2.366025403784441927 ) ) ;
#2986 = CARTESIAN_POINT ( 'NONE',  ( -62.99999999999998579, 8.614583332650536107, 2.077350269189627952 ) ) ;
#2987 = SURFACE_SIDE_STYLE ('',( #9874 ) ) ;
#2988 = CARTESIAN_POINT ( 'NONE',  ( 0.000000000000000000, -2.500000000000000000, 3.000000000000000000 ) ) ;
#2989 = CARTESIAN_POINT ( 'NONE',  ( -62.99999999999998579, 10.11458333265053611, 2.077350269189627952 ) ) ;
#2990 = ORIENTED_EDGE ( 'NONE', *, *, #1631, .F. ) ;
#2991 = AXIS2_PLACEMENT_3D ( 'NONE', #2140, #2079, #2196 ) ;
#2992 = DIRECTION ( 'NONE',  ( 0.000000000000000000, 0.000000000000000000, 1.000000000000000000 ) ) ;
#2993 = CARTESIAN_POINT ( 'NONE',  ( -62.43234176562498305, 13.16145833299193413, 0.7511620957034662593 ) ) ;
#2994 = VERTEX_POINT ( 'NONE', #9356 ) ;
#2995 = EDGE_CURVE ( 'NONE', #9106, #8034, #6093, .T. ) ;
#2996 = VECTOR ( 'NONE', #5662, 1000.000000000000000 ) ;
#2997 = CARTESIAN_POINT ( 'NONE',  ( -61.13531646874998415, 10.36979166632526805, 1.999225269531026417 ) ) ;
#2998 = DIRECTION ( 'NONE',  ( 0.000000000000000000, -1.084202172485504434E-16, 1.000000000000000000 ) ) ;
#2999 = CIRCLE ( 'NONE', #1404, 1.099999999999989875 ) ;
#3000 = CARTESIAN_POINT ( 'NONE',  ( -61.13531646874998415, 15.61979166632526628, 1.999225269531026417 ) ) ;
#3001 = FACE_OUTER_BOUND ( 'NONE', #5813, .T. ) ;
#3002 = VERTEX_POINT ( 'NONE', #81 ) ;
#3003 = CARTESIAN_POINT ( 'NONE',  ( 150.0000000000000000, -8.000000000000000000, 6.000000000000000000 ) ) ;
#3004 = MECHANICAL_DESIGN_GEOMETRIC_PRESENTATION_REPRESENTATION (  '', ( #6552 ), #5273 ) ;
#3005 = VECTOR ( 'NONE', #680, 1000.000000000000000 ) ;
#3006 = EDGE_LOOP ( 'NONE', ( #554, #2811 ) ) ;
#3007 = CARTESIAN_POINT ( 'NONE',  ( 0.5000000000000000000, 0.000000000000000000, 0.000000000000000000 ) ) ;
#3008 = CARTESIAN_POINT ( 'NONE',  ( -61.99999999999998579, 9.312500000000001776, 0.3452994616207497591 ) ) ;
#3009 = DIRECTION ( 'NONE',  ( -0.000000000000000000, -0.000000000000000000, -1.000000000000000000 ) ) ;
#3010 = CARTESIAN_POINT ( 'NONE',  ( -61.99999999999998579, 9.890624999658601979, 0.5015494609379544944 ) ) ;
#3011 = CARTESIAN_POINT ( 'NONE',  ( -62.99999999999998579, 8.322916665983870033, 0.9226497308103756012 ) ) ;
#3012 = CARTESIAN_POINT ( 'NONE',  ( -61.13531646874998415, 11.36979166632526628, 1.999225269531026417 ) ) ;
#3013 = CARTESIAN_POINT ( 'NONE',  ( -49.99999999999998579, -2.500000000000000000, 3.000000000000000000 ) ) ;
#3014 = ORIENTED_EDGE ( 'NONE', *, *, #10500, .T. ) ;
#3015 = DIRECTION ( 'NONE',  ( 0.000000000000000000, -0.000000000000000000, 1.000000000000000000 ) ) ;
#3016 = EDGE_CURVE ( 'NONE', #6871, #1245, #1161, .T. ) ;
#3017 = LINE ( 'NONE', #1299, #934 ) ;
#3018 = AXIS2_PLACEMENT_3D ( 'NONE', #10948, #173, #10335 ) ;
#3019 = ORIENTED_EDGE ( 'NONE', *, *, #2951, .F. ) ;
#3020 = CARTESIAN_POINT ( 'NONE',  ( -61.99999999999998579, 10.40624999931720218, 2.500000000000002665 ) ) ;
#3021 = CARTESIAN_POINT ( 'NONE',  ( -62.43234176562499016, 14.49479166632526983, 2.248837904296538071 ) ) ;
#3022 = CARTESIAN_POINT ( 'NONE',  ( -61.13531646874998415, 10.32812499965860198, 1.500000000000002220 ) ) ;
#3023 = MECHANICAL_DESIGN_GEOMETRIC_PRESENTATION_REPRESENTATION (  '', ( #8172 ), #6581 ) ;
#3024 = CARTESIAN_POINT ( 'NONE',  ( -37.99999999999999289, -14.00000000000000888, -0.9999999999999947820 ) ) ;
#3025 =( BOUNDED_CURVE ( )  B_SPLINE_CURVE ( 2, ( #8341, #5619, #3219, #6628, #9957, #9852, #7401, #3280, #10782 ),
 .UNSPECIFIED., .F., .T. ) 
 B_SPLINE_CURVE_WITH_KNOTS ( ( 3, 2, 2, 2, 3 ),
 ( 0.6796875000000000000, 0.6822916666666666297, 0.6875000000000000000, 0.6927083333333333703, 0.6953125000000000000 ),
 .UNSPECIFIED. ) 
 CURVE ( )  GEOMETRIC_REPRESENTATION_ITEM ( )  RATIONAL_B_SPLINE_CURVE ( ( 0.9330127018922194093, 0.9330127018922194093, 1.000000000000000000, 0.8660254037844387076, 1.000000000000000000, 0.8660254037844387076, 1.000000000000000000, 0.9330127018922194093, 0.9330127018922194093 ) ) 
 REPRESENTATION_ITEM ( '' )  );
#3026 = ORIENTED_EDGE ( 'NONE', *, *, #1748, .T. ) ;
#3027 = CARTESIAN_POINT ( 'NONE',  ( -61.99999999999998579, 14.81250000000000000, 0.5000000000000013323 ) ) ;
#3028 = CARTESIAN_POINT ( 'NONE',  ( -62.86468353124999453, 10.78645833299193413, 1.999225269531025750 ) ) ;
#3029 = PRODUCT_CONTEXT ( 'NONE', #1935, 'mechanical' ) ;
#3030 = CARTESIAN_POINT ( 'NONE',  ( -62.49999999999998579, 15.08333333333333393, 0.6339745962155627357 ) ) ;
#3031 = AXIS2_PLACEMENT_3D ( 'NONE', #9664, #9718, #6998 ) ;
#3032 = CARTESIAN_POINT ( 'NONE',  ( -62.99999999999998579, 14.11458333265053433, 2.077350269189627952 ) ) ;
#3033 = CARTESIAN_POINT ( 'NONE',  ( -61.99999999999998579, 16.00000000000000000, 2.500000000000000444 ) ) ;
#3034 = ORIENTED_EDGE ( 'NONE', *, *, #2793, .F. ) ;
#3035 = FACE_OUTER_BOUND ( 'NONE', #1234, .T. ) ;
#3036 = ORIENTED_EDGE ( 'NONE', *, *, #7473, .T. ) ;
#3037 = VERTEX_POINT ( 'NONE', #5321 ) ;
#3038 = CARTESIAN_POINT ( 'NONE',  ( -61.56765823437498142, 12.61979166632526805, 0.7511620957034663704 ) ) ;
#3039 = CARTESIAN_POINT ( 'NONE',  ( -61.56765823437498142, 9.119791666325268054, 0.7511620957034663704 ) ) ;
#3040 = LINE ( 'NONE', #9033, #9793 ) ;
#3041 = ORIENTED_EDGE ( 'NONE', *, *, #3250, .T. ) ;
#3042 = CARTESIAN_POINT ( 'NONE',  ( -60.99999999999998579, 12.72916666666666785, 2.077350269189628840 ) ) ;
#3043 = FACE_OUTER_BOUND ( 'NONE', #480, .T. ) ;
#3044 = CARTESIAN_POINT ( 'NONE',  ( -61.99999999999998579, 10.40624999931720396, 2.654700538379254571 ) ) ;
#3045 = EDGE_CURVE ( 'NONE', #9310, #5427, #7645, .T. ) ;
#3046 = ORIENTED_EDGE ( 'NONE', *, *, #7638, .F. ) ;
#3047 = FACE_OUTER_BOUND ( 'NONE', #2127, .T. ) ;
#3048 = CARTESIAN_POINT ( 'NONE',  ( -62.86468353124998742, 12.72395833299193413, 1.999225269531025972 ) ) ;
#3049 = CARTESIAN_POINT ( 'NONE',  ( 0.05007909176323187272, -0.2500000000000000000, 1.595164775286565861 ) ) ;
#3050 = ORIENTED_EDGE ( 'NONE', *, *, #1928, .F. ) ;
#3051 = CARTESIAN_POINT ( 'NONE',  ( -61.56765823437498852, 11.84895833299193413, 2.248837904296538515 ) ) ;
#3052 = FACE_OUTER_BOUND ( 'NONE', #10804, .T. ) ;
#3053 = CIRCLE ( 'NONE', #1453, 1.000000000000000000 ) ;
#3054 = CARTESIAN_POINT ( 'NONE',  ( -61.99999999999998579, 15.20312499965860020, 0.5015494609379544944 ) ) ;
#3055 = VERTEX_POINT ( 'NONE', #9414 ) ;
#3056 = DIRECTION ( 'NONE',  ( -0.000000000000000000, -1.000000000000000000, -0.000000000000000000 ) ) ;
#3057 = EDGE_CURVE ( 'NONE', #484, #4783, #30, .T. ) ;
#3058 = AXIS2_PLACEMENT_3D ( 'NONE', #6518, #9069, #7400 ) ;
#3059 = ORIENTED_EDGE ( 'NONE', *, *, #3852, .F. ) ;
#3060 = DIRECTION ( 'NONE',  ( -0.7071067811865439090, 0.000000000000000000, -0.7071067811865512365 ) ) ;
#3061 = CARTESIAN_POINT ( 'NONE',  ( -62.99999999999998579, 9.104166666666666075, 0.9226497308103756012 ) ) ;
#3062 = PLANE ( 'NONE',  #6813 ) ;
#3063 = CARTESIAN_POINT ( 'NONE',  ( -61.99999999999998579, 16.00000000000000000, 2.500000000000000444 ) ) ;
#3064 = DIRECTION ( 'NONE',  ( -0.000000000000000000, -1.000000000000000000, -0.000000000000000000 ) ) ;
#3065 = CARTESIAN_POINT ( 'NONE',  ( -60.99999999999998579, 15.44791666598387003, 2.077350269189628840 ) ) ;
#3066 = AXIS2_PLACEMENT_3D ( 'NONE', #5324, #2233, #2335 ) ;
#3067 = CARTESIAN_POINT ( 'NONE',  ( -62.86468353124998032, 12.24479166632526805, 1.000774730468978246 ) ) ;
#3068 = CARTESIAN_POINT ( 'NONE',  ( -62.49999999999998579, 13.66666666666666785, 2.366025403784441483 ) ) ;
#3069 = ORIENTED_EDGE ( 'NONE', *, *, #8889, .T. ) ;
#3070 = LINE ( 'NONE', #9849, #4080 ) ;
#3071 = CARTESIAN_POINT ( 'NONE',  ( 145.0000000000000284, 5.500000000000000000, 3.000000000000000000 ) ) ;
#3072 = VERTEX_POINT ( 'NONE', #5661 ) ;
#3073 = DIRECTION ( 'NONE',  ( -1.000000000000000000, 0.000000000000000000, 0.000000000000000000 ) ) ;
#3074 = CARTESIAN_POINT ( 'NONE',  ( -61.56765823437498852, 13.53645833299193413, 2.248837904296538515 ) ) ;
#3075 = CARTESIAN_POINT ( 'NONE',  ( -62.86468353124999453, 9.703124999658601979, 1.500000000000002220 ) ) ;
#3076 = LINE ( 'NONE', #416, #2445 ) ;
#3077 = ORIENTED_EDGE ( 'NONE', *, *, #2902, .T. ) ;
#3078 = CARTESIAN_POINT ( 'NONE',  ( -31.99999999999997868, -14.00000000000000888, -0.9999999999999947820 ) ) ;
#3079 = CARTESIAN_POINT ( 'NONE',  ( -61.13531646874997705, 11.86979166632526805, 1.999225269531026417 ) ) ;
#3080 = APPLICATION_PROTOCOL_DEFINITION ( 'draft international standard', 'automotive_design', 1998, #233 ) ;
#3081 = PLANE ( 'NONE',  #6384 ) ;
#3082 = CARTESIAN_POINT ( 'NONE',  ( -61.99999999999998579, 15.78124999931720218, 0.3452994616207497591 ) ) ;
#3083 = CARTESIAN_POINT ( 'NONE',  ( -61.28647452029539267, 16.00000000000000000, 0.7993707187018740390 ) ) ;
#3084 = ORIENTED_EDGE ( 'NONE', *, *, #4899, .F. ) ;
#3085 = CIRCLE ( 'NONE', #433, 1.000000000000000888 ) ;
#3086 = VERTEX_POINT ( 'NONE', #5179 ) ;
#3087 = EDGE_CURVE ( 'NONE', #7723, #1190, #3467, .T. ) ;
#3088 =( BOUNDED_CURVE ( )  B_SPLINE_CURVE ( 2, ( #9450, #3618, #7014, #2789, #1847, #1121, #6177, #10218, #4503 ),
 .UNSPECIFIED., .F., .T. ) 
 B_SPLINE_CURVE_WITH_KNOTS ( ( 3, 2, 2, 2, 3 ),
 ( 0.4140625000000000000, 0.4166666666666666852, 0.4218750000000000000, 0.4270833333333333148, 0.4296875000000000555 ),
 .UNSPECIFIED. ) 
 CURVE ( )  GEOMETRIC_REPRESENTATION_ITEM ( )  RATIONAL_B_SPLINE_CURVE ( ( 0.9330127018922194093, 0.9330127018922194093, 1.000000000000000000, 0.8660254037844387076, 1.000000000000000000, 0.8660254037844387076, 1.000000000000000000, 0.9330127018922178550, 0.9330127018922192983 ) ) 
 REPRESENTATION_ITEM ( '' )  );
#3089 = CARTESIAN_POINT ( 'NONE',  ( -62.43234176562499016, 12.74479166632526805, 2.248837904296538071 ) ) ;
#3090 = CARTESIAN_POINT ( 'NONE',  ( -61.13531646874998415, 10.30729166632526805, 1.999225269531026417 ) ) ;
#3091 = CARTESIAN_POINT ( 'NONE',  ( -61.49999999999998579, 11.79166666666666785, 0.6339745962155628467 ) ) ;
#3092 = ORIENTED_EDGE ( 'NONE', *, *, #6873, .F. ) ;
#3093 = CARTESIAN_POINT ( 'NONE',  ( -62.99999999999998579, 14.14583333333333215, 2.077350269189627952 ) ) ;
#3094 = EDGE_CURVE ( 'NONE', #9315, #7434, #8946, .T. ) ;
#3095 = FACE_OUTER_BOUND ( 'NONE', #10378, .T. ) ;
#3096 =( NAMED_UNIT ( * ) PLANE_ANGLE_UNIT ( ) SI_UNIT ( $, .RADIAN. ) );
#3097 = CARTESIAN_POINT ( 'NONE',  ( -61.99999999999998579, 11.40624999931720218, 2.654700538379254571 ) ) ;
#3098 = CARTESIAN_POINT ( 'NONE',  ( 0.5000000000000000000, 2.361209666477099964E-16, -1.928074011315806136 ) ) ;
#3099 = CARTESIAN_POINT ( 'NONE',  ( -61.13531646874998415, 13.09895833299193413, 1.000774730468978468 ) ) ;
#3100 = ORIENTED_EDGE ( 'NONE', *, *, #5058, .F. ) ;
#3101 = CARTESIAN_POINT ( 'NONE',  ( -61.99999999999998579, 11.20312499965860198, 0.5015494609379544944 ) ) ;
#3102 = CARTESIAN_POINT ( 'NONE',  ( -62.49999999999998579, 12.63541666598386826, 2.366025403784441483 ) ) ;
#3103 = CARTESIAN_POINT ( 'NONE',  ( 0.5000000000000000000, 0.2499999999999982792, 1.911797424705720339 ) ) ;
#3104 = VERTEX_POINT ( 'NONE', #1499 ) ;
#3105 = DIRECTION ( 'NONE',  ( -0.000000000000000000, 0.000000000000000000, 1.000000000000000000 ) ) ;
#3106 = ADVANCED_FACE ( 'NONE', ( #4642 ), #1821, .T. ) ;
#3107 = EDGE_CURVE ( 'NONE', #8537, #8097, #10412, .T. ) ;
#3108 = ORIENTED_EDGE ( 'NONE', *, *, #5529, .T. ) ;
#3109 = CARTESIAN_POINT ( 'NONE',  ( -61.73205080756885366, 9.520085449632571084, 0.5000000000000028866 ) ) ;
#3110 = CARTESIAN_POINT ( 'NONE',  ( -61.99999999999998579, 9.937500000000001776, 2.654700538379254571 ) ) ;
#3111 = CARTESIAN_POINT ( 'NONE',  ( -60.99999999999998579, 11.25000000000000000, 1.500000000000002220 ) ) ;
#3112 = CARTESIAN_POINT ( 'NONE',  ( -60.99999999999998579, 16.21874999931720396, 1.500000000000002220 ) ) ;
#3113 =( BOUNDED_CURVE ( )  B_SPLINE_CURVE ( 2, ( #6042, #3372, #2431, #9232, #2596, #6718, #9270, #4200, #10252 ),
 .UNSPECIFIED., .F., .F. ) 
 B_SPLINE_CURVE_WITH_KNOTS ( ( 3, 2, 2, 2, 3 ),
 ( 0.2734375000000000000, 0.2760416666666666852, 0.2812500000000000000, 0.2864583333333333148, 0.2890624999999999445 ),
 .UNSPECIFIED. ) 
 CURVE ( )  GEOMETRIC_REPRESENTATION_ITEM ( )  RATIONAL_B_SPLINE_CURVE ( ( 0.9330127018922194093, 0.9330127018922194093, 1.000000000000000000, 0.8660254037844387076, 1.000000000000000000, 0.8660254037844387076, 1.000000000000000000, 0.9330127018922207416, 0.9330127018922192983 ) ) 
 REPRESENTATION_ITEM ( '' )  );
#3114 = CARTESIAN_POINT ( 'NONE',  ( -139.9999999999999716, -8.000000000000000000, 0.000000000000000000 ) ) ;
#3115 = CARTESIAN_POINT ( 'NONE',  ( -61.49999999999998579, 8.260416665983870033, 0.6339745962155628467 ) ) ;
#3116 = CARTESIAN_POINT ( 'NONE',  ( -61.13531646874998415, 11.86979166632526805, 1.999225269531026417 ) ) ;
#3117 = DIRECTION ( 'NONE',  ( 0.8660254037844418162, -0.4999999999999947264, 0.000000000000000000 ) ) ;
#3118 = PRODUCT_DEFINITION ( 'UNKNOWN', '', #7460, #8348 ) ;
#3119 = EDGE_LOOP ( 'NONE', ( #9591, #7980, #8165, #6395 ) ) ;
#3120 = CARTESIAN_POINT ( 'NONE',  ( -49.99999999999998579, 8.000000000000000000, 3.000000000000000000 ) ) ;
#3121 = CARTESIAN_POINT ( 'NONE',  ( 140.0000000000000284, -8.000000000000000000, 6.000000000000000000 ) ) ;
#3122 = CYLINDRICAL_SURFACE ( 'NONE', #3058, 1.000000000000000888 ) ;
#3123 = DIRECTION ( 'NONE',  ( 0.000000000000000000, 0.000000000000000000, -1.000000000000000000 ) ) ;
#3124 = CARTESIAN_POINT ( 'NONE',  ( -62.86468353124998032, 13.43229166632526628, 1.000774730468978246 ) ) ;
#3125 = CARTESIAN_POINT ( 'NONE',  ( -62.86468353124998032, 10.18229166632526805, 1.000774730468978024 ) ) ;
#3126 = CARTESIAN_POINT ( 'NONE',  ( 150.0000000000000284, -2.500000000000000000, 2.000000000000000000 ) ) ;
#3127 = VERTEX_POINT ( 'NONE', #10473 ) ;
#3128 = CARTESIAN_POINT ( 'NONE',  ( -61.99999999999998579, 12.28124999931720041, 0.5000000000000013323 ) ) ;
#3129 = CARTESIAN_POINT ( 'NONE',  ( -61.13531646874997705, 11.16145833299193413, 1.000774730468978468 ) ) ;
#3130 = EDGE_CURVE ( 'NONE', #9717, #4004, #7034, .T. ) ;
#3131 = CARTESIAN_POINT ( 'NONE',  ( -61.99999999999998579, 16.07812499965860198, 2.498450539062049724 ) ) ;
#3132 = ITEM_DEFINED_TRANSFORMATION ( 'NONE', 'NONE', #4241,  #2307 ) ;
#3133 = CARTESIAN_POINT ( 'NONE',  ( -62.99999999999998579, 15.12500000000000000, 1.500000000000001998 ) ) ;
#3134 = CARTESIAN_POINT ( 'NONE',  ( -62.49999999999998579, 15.63541666598386826, 2.366025403784441483 ) ) ;
#3135 = DIRECTION ( 'NONE',  ( 1.000000000000000000, 0.000000000000000000, 0.000000000000000000 ) ) ;
#3136 = ORIENTED_EDGE ( 'NONE', *, *, #6578, .F. ) ;
#3137 = CARTESIAN_POINT ( 'NONE',  ( -62.99999999999998579, 11.82291666598387003, 0.9226497308103756012 ) ) ;
#3138 = DIRECTION ( 'NONE',  ( 0.000000000000000000, -0.000000000000000000, 1.000000000000000000 ) ) ;
#3139 = CARTESIAN_POINT ( 'NONE',  ( -61.56765823437498852, 14.28645833299193413, 2.248837904296538515 ) ) ;
#3140 = CARTESIAN_POINT ( 'NONE',  ( -62.86468353124998032, 10.43229166632526983, 1.000774730468978246 ) ) ;
#3141 = CARTESIAN_POINT ( 'NONE',  ( -114.9999999999999289, -7.999999999999998224, -2.000000000000000000 ) ) ;
#3142 = ORIENTED_EDGE ( 'NONE', *, *, #4091, .T. ) ;
#3143 = CARTESIAN_POINT ( 'NONE',  ( -60.99999999999998579, 13.25000000000000000, 1.500000000000002220 ) ) ;
#3144 = CARTESIAN_POINT ( 'NONE',  ( -61.99999999999998579, 8.656249999317202182, 2.500000000000002665 ) ) ;
#3145 = EDGE_CURVE ( 'NONE', #6502, #4541, #308, .T. ) ;
#3146 = FILL_AREA_STYLE_COLOUR ( '', #7452 ) ;
#3147 = CARTESIAN_POINT ( 'NONE',  ( -60.99999999999998579, 11.46874999931720218, 1.500000000000002220 ) ) ;
#3148 = CARTESIAN_POINT ( 'NONE',  ( -62.26794919243111082, 14.82366454968463287, 0.5000000000000013323 ) ) ;
#3149 = EDGE_CURVE ( 'NONE', #10303, #7043, #5412, .T. ) ;
#3150 = CARTESIAN_POINT ( 'NONE',  ( -61.56765823437498142, 14.36979166632526983, 0.7511620957034663704 ) ) ;
#3151 = FILL_AREA_STYLE ('',( #1588 ) ) ;
#3152 = VERTEX_POINT ( 'NONE', #6199 ) ;
#3153 = CARTESIAN_POINT ( 'NONE',  ( -61.13531646874998415, 11.11979166632526805, 1.999225269531026417 ) ) ;
#3154 = DIRECTION ( 'NONE',  ( 0.000000000000000000, -1.000000000000000000, 0.000000000000000000 ) ) ;
#3155 = CARTESIAN_POINT ( 'NONE',  ( -62.86468353124998032, 15.24479166632526805, 1.000774730468978246 ) ) ;
#3156 = ORIENTED_EDGE ( 'NONE', *, *, #4861, .T. ) ;
#3157 = LINE ( 'NONE', #8320, #551 ) ;
#3158 = VERTEX_POINT ( 'NONE', #3693 ) ;
#3159 = DIRECTION ( 'NONE',  ( 0.000000000000000000, 0.000000000000000000, -1.000000000000000000 ) ) ;
#3160 = CARTESIAN_POINT ( 'NONE',  ( -62.99999999999998579, 9.604166666666667851, 0.9226497308103756012 ) ) ;
#3161 = CARTESIAN_POINT ( 'NONE',  ( -62.26794919243111082, 12.92633545031537068, 2.500000000000003109 ) ) ;
#3162 = AXIS2_PLACEMENT_3D ( 'NONE', #7005, #3782, #8011 ) ;
#3163 = CARTESIAN_POINT ( 'NONE',  ( -61.56765823437498142, 8.182291666325268054, 0.7511620957034663704 ) ) ;
#3164 = CARTESIAN_POINT ( 'NONE',  ( -62.49999999999998579, 15.80208333265053788, 0.6339745962155627357 ) ) ;
#3165 = AXIS2_PLACEMENT_3D ( 'NONE', #5496, #10498, #10557 ) ;
#3166 = CARTESIAN_POINT ( 'NONE',  ( -61.56765823437498852, 12.09895833299193413, 2.248837904296538515 ) ) ;
#3167 = EDGE_CURVE ( 'NONE', #8229, #5900, #9987, .T. ) ;
#3168 = CARTESIAN_POINT ( 'NONE',  ( -61.99999999999998579, 9.156249999317203958, 2.500000000000002665 ) ) ;
#3169 = ORIENTED_EDGE ( 'NONE', *, *, #5271, .T. ) ;
#3170 = CARTESIAN_POINT ( 'NONE',  ( -60.99999999999998579, 9.218749999317203958, 1.500000000000002220 ) ) ;
#3171 = AXIS2_PLACEMENT_3D ( 'NONE', #861, #10972, #4243 ) ;
#3172 = FACE_OUTER_BOUND ( 'NONE', #10185, .T. ) ;
#3173 = FACE_OUTER_BOUND ( 'NONE', #1689, .T. ) ;
#3174 = CARTESIAN_POINT ( 'NONE',  ( -61.99999999999998579, 14.26562499965860020, 2.498450539062049724 ) ) ;
#3175 = DIRECTION ( 'NONE',  ( 1.000000000000000000, 0.000000000000000000, 0.000000000000000000 ) ) ;
#3176 = CARTESIAN_POINT ( 'NONE',  ( 150.0000000000000000, 8.000000000000000000, 6.000000000000000000 ) ) ;
#3177 = DIRECTION ( 'NONE',  ( 1.000000000000000000, 0.000000000000000000, 0.000000000000000000 ) ) ;
#3178 = CARTESIAN_POINT ( 'NONE',  ( -62.86468353124998032, 10.99479166632526628, 1.000774730468978024 ) ) ;
#3179 = CARTESIAN_POINT ( 'NONE',  ( -62.43234176562498305, 15.72395833299193590, 0.7511620957034662593 ) ) ;
#3180 = CIRCLE ( 'NONE', #4398, 25.99999999999999645 ) ;
#3181 = APPLICATION_PROTOCOL_DEFINITION ( 'draft international standard', 'automotive_design', 1998, #9523 ) ;
#3182 = FACE_OUTER_BOUND ( 'NONE', #5830, .T. ) ;
#3183 = CARTESIAN_POINT ( 'NONE',  ( -60.99999999999998579, 15.46874999931720218, 1.500000000000002220 ) ) ;
#3184 = DIRECTION ( 'NONE',  ( -1.000000000000000000, -0.000000000000000000, -0.000000000000000000 ) ) ;
#3185 = ORIENTED_EDGE ( 'NONE', *, *, #5664, .T. ) ;
#3186 = CARTESIAN_POINT ( 'NONE',  ( -61.99999999999997868, 8.281249999317202182, 0.5000000000000013323 ) ) ;
#3187 = CARTESIAN_POINT ( 'NONE',  ( -62.49999999999998579, 12.66666666666666607, 2.366025403784441483 ) ) ;
#3188 = AXIS2_PLACEMENT_3D ( 'NONE', #1571, #10797, #8356 ) ;
#3189 = EDGE_CURVE ( 'NONE', #4004, #7100, #8044, .T. ) ;
#3190 = PRESENTATION_LAYER_ASSIGNMENT (  '', '', ( #1765 ) ) ;
#3191 = CARTESIAN_POINT ( 'NONE',  ( -61.13531646874997705, 14.30729166632526983, 1.999225269531026417 ) ) ;
#3192 = CARTESIAN_POINT ( 'NONE',  ( -61.99999999999998579, 9.265624999658600203, 2.498450539062049724 ) ) ;
#3193 = CARTESIAN_POINT ( 'NONE',  ( -60.99999999999998579, 14.44791666598387003, 2.077350269189628840 ) ) ;
#3194 = VERTEX_POINT ( 'NONE', #9649 ) ;
#3195 = CARTESIAN_POINT ( 'NONE',  ( -61.99999999999998579, 13.81249999999999822, 0.3452994616207497591 ) ) ;
#3196 = CARTESIAN_POINT ( 'NONE',  ( -60.99999999999998579, 8.979166666666666075, 2.077350269189628840 ) ) ;
#3197 = VECTOR ( 'NONE', #5882, 1000.000000000000000 ) ;
#3198 = SURFACE_STYLE_FILL_AREA ( #7579 ) ;
#3199 = CARTESIAN_POINT ( 'NONE',  ( -62.99999999999998579, 12.34374999931720218, 1.500000000000001998 ) ) ;
#3200 = CARTESIAN_POINT ( 'NONE',  ( -60.99999999999998579, 9.520833333333333925, 0.9226497308103762673 ) ) ;
#3201 = CARTESIAN_POINT ( 'NONE',  ( -62.43234176562499016, 14.49479166632526983, 2.248837904296538071 ) ) ;
#3202 = CARTESIAN_POINT ( 'NONE',  ( -61.49999999999998579, 11.45833333333333393, 2.366025403784441927 ) ) ;
#3203 = ORIENTED_EDGE ( 'NONE', *, *, #2239, .T. ) ;
#3204 = CARTESIAN_POINT ( 'NONE',  ( -62.43234176562499016, 12.05729166632526628, 2.248837904296538071 ) ) ;
#3205 = DIRECTION ( 'NONE',  ( 0.000000000000000000, 0.000000000000000000, -1.000000000000000000 ) ) ;
#3206 = CARTESIAN_POINT ( 'NONE',  ( -62.43234176562499016, 15.30729166632526805, 2.248837904296538071 ) ) ;
#3207 = ORIENTED_EDGE ( 'NONE', *, *, #3571, .T. ) ;
#3208 = DIRECTION ( 'NONE',  ( -0.000000000000000000, -1.000000000000000000, -0.000000000000000000 ) ) ;
#3209 = ORIENTED_EDGE ( 'NONE', *, *, #5754, .T. ) ;
#3210 = CARTESIAN_POINT ( 'NONE',  ( -61.49999999999998579, 9.708333333333332149, 2.366025403784441927 ) ) ;
#3211 = CARTESIAN_POINT ( 'NONE',  ( -61.73205080756886787, 8.551335450315370679, 0.5000000000000036637 ) ) ;
#3212 = CYLINDRICAL_SURFACE ( 'NONE', #6186, 0.9999999999999981126 ) ;
#3213 = ADVANCED_FACE ( 'NONE', ( #9587 ), #4525, .T. ) ;
#3214 = CARTESIAN_POINT ( 'NONE',  ( -57.99999999999998579, -10.00000000000000888, 3.000000000000000000 ) ) ;
#3215 = CARTESIAN_POINT ( 'NONE',  ( -61.99999999999998579, 11.82812499965860198, 2.498450539062049724 ) ) ;
#3216 = ORIENTED_EDGE ( 'NONE', *, *, #6767, .T. ) ;
#3217 = CARTESIAN_POINT ( 'NONE',  ( 150.0000000000000284, -2.500000000000000000, 4.000000000000000000 ) ) ;
#3218 = DIRECTION ( 'NONE',  ( 1.000000000000000000, 0.000000000000000000, -0.000000000000000000 ) ) ;
#3219 = CARTESIAN_POINT ( 'NONE',  ( -61.49999999999998579, 13.67708333265053433, 2.366025403784441927 ) ) ;
#3220 = CARTESIAN_POINT ( 'NONE',  ( -62.86468353124998032, 13.93229166632526805, 1.000774730468978246 ) ) ;
#3221 = EDGE_CURVE ( 'NONE', #381, #2581, #8403, .T. ) ;
#3222 = DIRECTION ( 'NONE',  ( -0.000000000000000000, -1.000000000000000000, -0.000000000000000000 ) ) ;
#3223 = CARTESIAN_POINT ( 'NONE',  ( -61.49999999999998579, 14.54166666666666607, 0.6339745962155628467 ) ) ;
#3224 = FACE_BOUND ( 'NONE', #1027, .T. ) ;
#3225 = AXIS2_PLACEMENT_3D ( 'NONE', #4880, #5720, #10931 ) ;
#3226 = CARTESIAN_POINT ( 'NONE',  ( -62.43234176562498305, 13.22395833299193413, 0.7511620957034662593 ) ) ;
#3227 = CARTESIAN_POINT ( 'NONE',  ( -61.13531646874998415, 15.86979166632526628, 1.999225269531026417 ) ) ;
#3228 = CARTESIAN_POINT ( 'NONE',  ( -61.99999999999997868, 8.062500000000000000, 0.5000000000000013323 ) ) ;
#3229 = ITEM_DEFINED_TRANSFORMATION ( 'NONE', 'NONE', #9223,  #2307 ) ;
#3230 = CARTESIAN_POINT ( 'NONE',  ( -62.49999999999998579, 15.16666666666666607, 2.366025403784441483 ) ) ;
#3231 = CARTESIAN_POINT ( 'NONE',  ( -62.43234176562499016, 8.307291666325268054, 2.248837904296538071 ) ) ;
#3232 = ORIENTED_EDGE ( 'NONE', *, *, #7753, .F. ) ;
#3233 = PLANE ( 'NONE',  #162 ) ;
#3234 = CARTESIAN_POINT ( 'NONE',  ( -76.99999999999998579, 11.49999999999999645, 5.000000000000000000 ) ) ;
#3235 =( BOUNDED_CURVE ( )  B_SPLINE_CURVE ( 2, ( #6354, #2857, #6243, #3800, #2194, #6417, #2023, #5572, #9741 ),
 .UNSPECIFIED., .F., .T. ) 
 B_SPLINE_CURVE_WITH_KNOTS ( ( 3, 2, 2, 2, 3 ),
 ( 0.07031249999999995837, 0.07291666666666667129, 0.07812500000000000000, 0.08333333333333332871, 0.08593750000000000000 ),
 .UNSPECIFIED. ) 
 CURVE ( )  GEOMETRIC_REPRESENTATION_ITEM ( )  RATIONAL_B_SPLINE_CURVE ( ( 0.9330127018922194093, 0.9330127018922182991, 1.000000000000000000, 0.8660254037844387076, 1.000000000000000000, 0.8660254037844387076, 1.000000000000000000, 0.9330127018922194093, 0.9330127018922194093 ) ) 
 REPRESENTATION_ITEM ( '' )  );
#3236 = AXIS2_PLACEMENT_3D ( 'NONE', #3517, #1860, #8635 ) ;
#3237 = ADVANCED_FACE ( 'NONE', ( #4579 ), #5237, .T. ) ;
#3238 = VECTOR ( 'NONE', #9626, 1000.000000000000000 ) ;
#3239 = CARTESIAN_POINT ( 'NONE',  ( -61.99999999999999289, 13.64062499965860198, 0.5015494609379544944 ) ) ;
#3240 = CARTESIAN_POINT ( 'NONE',  ( -61.56765823437498852, 9.286458332991935904, 2.248837904296538515 ) ) ;
#3241 = ADVANCED_FACE ( 'NONE', ( #9702 ), #6981, .F. ) ;
#3242 = CARTESIAN_POINT ( 'NONE',  ( -62.86468353124999453, 16.01562499965860198, 1.500000000000002220 ) ) ;
#3243 = DIRECTION ( 'NONE',  ( -1.000000000000000000, 0.000000000000000000, 0.000000000000000000 ) ) ;
#3244 = ORIENTED_EDGE ( 'NONE', *, *, #4320, .T. ) ;
#3245 = CARTESIAN_POINT ( 'NONE',  ( -60.99999999999998579, 13.27083333333333215, 0.9226497308103762673 ) ) ;
#3246 = PRODUCT_DEFINITION_SHAPE ( 'NONE', 'NONE',  #5895 ) ;
#3247 = CARTESIAN_POINT ( 'NONE',  ( -62.86468353124999453, 9.286458332991934128, 1.999225269531025750 ) ) ;
#3248 = SURFACE_STYLE_USAGE ( .BOTH. , #2468 ) ;
#3249 = AXIS2_PLACEMENT_3D ( 'NONE', #345, #8964, #9795 ) ;
#3250 = EDGE_CURVE ( 'NONE', #9814, #2202, #8336, .T. ) ;
#3251 = CARTESIAN_POINT ( 'NONE',  ( -61.99999999999998579, 11.65624999931720218, 2.654700538379254571 ) ) ;
#3252 = CARTESIAN_POINT ( 'NONE',  ( 190.0000000000000000, -6.123233995736783046E-16, 2.000000000000000000 ) ) ;
#3253 = PRODUCT_DEFINITION ( 'UNKNOWN', '', #7291, #4620 ) ;
#3254 = AXIS2_PLACEMENT_3D ( 'NONE', #8554, #10436, #9493 ) ;
#3255 = CARTESIAN_POINT ( 'NONE',  ( -62.86468353124998742, 14.22395833299193590, 1.999225269531025972 ) ) ;
#3256 = SURFACE_STYLE_USAGE ( .BOTH. , #8370 ) ;
#3257 = ORIENTED_EDGE ( 'NONE', *, *, #5403, .F. ) ;
#3258 = CARTESIAN_POINT ( 'NONE',  ( -62.86468353124998032, 12.24479166632526805, 1.000774730468978246 ) ) ;
#3259 = CYLINDRICAL_SURFACE ( 'NONE', #2299, 0.9999999999999981126 ) ;
#3260 = EDGE_CURVE ( 'NONE', #381, #3952, #10359, .T. ) ;
#3261 = FACE_BOUND ( 'NONE', #3740, .T. ) ;
#3262 = ORIENTED_EDGE ( 'NONE', *, *, #7252, .F. ) ;
#3263 = CARTESIAN_POINT ( 'NONE',  ( -61.99999999999998579, 14.68750000000000000, 2.500000000000002665 ) ) ;
#3264 = B_SPLINE_CURVE_WITH_KNOTS ( 'NONE', 3,
 ( #213, #3599, #6160, #4486, #7892, #270 ),
 .UNSPECIFIED., .F., .F.,
 ( 4, 2, 4 ),
 ( 0.003549988921687060456, 0.003971677118101641160, 0.004393365314516220997 ),
 .UNSPECIFIED. ) ;
#3265 = EDGE_CURVE ( 'NONE', #4030, #6875, #8059, .T. ) ;
#3266 = EDGE_LOOP ( 'NONE', ( #5242, #10695, #6445, #4094 ) ) ;
#3267 = CARTESIAN_POINT ( 'NONE',  ( -61.73205080756884655, 8.667414549001829727, 2.500000000000004885 ) ) ;
#3268 = CARTESIAN_POINT ( 'NONE',  ( -60.99999999999998579, 11.47916666666666607, 2.077350269189628840 ) ) ;
#3269 = DIRECTION ( 'NONE',  ( -0.000000000000000000, -1.000000000000000000, -0.000000000000000000 ) ) ;
#3270 = LINE ( 'NONE', #4151, #4043 ) ;
#3271 = UNCERTAINTY_MEASURE_WITH_UNIT (LENGTH_MEASURE( 1.000000000000000082E-05 ), #2442, 'distance_accuracy_value', 'NONE');
#3272 = EDGE_CURVE ( 'NONE', #7919, #7344, #9179, .T. ) ;
#3273 = CARTESIAN_POINT ( 'NONE',  ( -61.49999999999998579, 8.677083332650536107, 2.366025403784441927 ) ) ;
#3274 = CARTESIAN_POINT ( 'NONE',  ( -62.86468353124999453, 13.76562499965860198, 1.500000000000002220 ) ) ;
#3275 = FACE_OUTER_BOUND ( 'NONE', #7656, .T. ) ;
#3276 = VERTEX_POINT ( 'NONE', #1376 ) ;
#3277 = CARTESIAN_POINT ( 'NONE',  ( -61.99999999999998579, 16.00000000000000000, 2.500000000000000444 ) ) ;
#3278 = EDGE_CURVE ( 'NONE', #10979, #7075, #10304, .T. ) ;
#3279 = EDGE_LOOP ( 'NONE', ( #2969, #10216, #1655, #1072 ) ) ;
#3280 = CARTESIAN_POINT ( 'NONE',  ( -61.73205080756886076, 13.77008544963257464, 0.5000000000000014433 ) ) ;
#3281 = CARTESIAN_POINT ( 'NONE',  ( -61.13531646874998415, 15.59895833299193590, 1.000774730468978468 ) ) ;
#3282 = CARTESIAN_POINT ( 'NONE',  ( -62.99999999999998579, 11.89583333333333215, 2.077350269189627952 ) ) ;
#3283 = CARTESIAN_POINT ( 'NONE',  ( -61.49999999999998579, 11.76041666598387003, 0.6339745962155628467 ) ) ;
#3284 = CYLINDRICAL_SURFACE ( 'NONE', #7591, 1.099999999999989875 ) ;
#3285 = CARTESIAN_POINT ( 'NONE',  ( -61.99999999999999289, 12.32812499965860198, 2.498450539062049724 ) ) ;
#3286 = CARTESIAN_POINT ( 'NONE',  ( -62.86468353124998742, 15.53645833299193590, 1.999225269531025972 ) ) ;
#3287 = CARTESIAN_POINT ( 'NONE',  ( -62.26794919243111082, 14.29241454900183328, 0.5000000000000013323 ) ) ;
#3288 = LINE ( 'NONE', #10269, #3704 ) ;
#3289 = CARTESIAN_POINT ( 'NONE',  ( -60.99999999999998579, 15.98958333265053433, 0.9226497308103762673 ) ) ;
#3290 = DIRECTION ( 'NONE',  ( -1.000000000000000000, -0.000000000000000000, -0.000000000000000000 ) ) ;
#3291 = VERTEX_POINT ( 'NONE', #4026 ) ;
#3292 = CARTESIAN_POINT ( 'NONE',  ( -62.26794919243111082, 11.79241454900183328, 0.5000000000000013323 ) ) ;
#3293 = DIRECTION ( 'NONE',  ( 1.000000000000000000, 0.000000000000000000, 0.000000000000000000 ) ) ;
#3294 = CARTESIAN_POINT ( 'NONE',  ( -61.99999999999999289, 13.89062499965860198, 0.5015494609379544944 ) ) ;
#3295 = CARTESIAN_POINT ( 'NONE',  ( -62.86468353124999453, 10.20312499965860198, 1.500000000000002220 ) ) ;
#3296 = CARTESIAN_POINT ( 'NONE',  ( -61.56765823437498142, 15.43229166632526805, 0.7511620957034663704 ) ) ;
#3297 = CARTESIAN_POINT ( 'NONE',  ( -61.99999999999998579, -15.00000000000001421, 2.500000000000003109 ) ) ;
#3298 = ORIENTED_EDGE ( 'NONE', *, *, #6350, .F. ) ;
#3299 = CARTESIAN_POINT ( 'NONE',  ( -62.49999999999998579, 13.16666666666666607, 2.366025403784441483 ) ) ;
#3300 = CARTESIAN_POINT ( 'NONE',  ( -61.99999999999999289, 8.953124999658601979, 0.5015494609379544944 ) ) ;
#3301 = ADVANCED_FACE ( 'NONE', ( #3095 ), #9817, .T. ) ;
#3302 = CARTESIAN_POINT ( 'NONE',  ( -62.99999999999998579, 12.11458333265053611, 2.077350269189627952 ) ) ;
#3303 =( BOUNDED_CURVE ( )  B_SPLINE_CURVE ( 2, ( #4545, #7951, #3721, #7119, #3112 ),
 .UNSPECIFIED., .F., .T. ) 
 B_SPLINE_CURVE_WITH_KNOTS ( ( 3, 2, 3 ),
 ( 0.9921875000000000000, 0.9947916666666666297, 1.000000000000000000 ),
 .UNSPECIFIED. ) 
 CURVE ( )  GEOMETRIC_REPRESENTATION_ITEM ( )  RATIONAL_B_SPLINE_CURVE ( ( 0.9330127018922194093, 0.9330127018922194093, 1.000000000000000000, 0.8660254037844387076, 1.000000000000000000 ) ) 
 REPRESENTATION_ITEM ( '' )  );
#3304 = CYLINDRICAL_SURFACE ( 'NONE', #8558, 1.000000000000000000 ) ;
#3305 = EDGE_CURVE ( 'NONE', #5709, #3086, #6491, .T. ) ;
#3306 = CARTESIAN_POINT ( 'NONE',  ( -62.43234176562498305, 13.66145833299193413, 0.7511620957034662593 ) ) ;
#3307 = ORIENTED_EDGE ( 'NONE', *, *, #8457, .T. ) ;
#3308 = CARTESIAN_POINT ( 'NONE',  ( -61.99999999999998579, 12.32812499965860376, 2.498450539062049724 ) ) ;
#3309 = CARTESIAN_POINT ( 'NONE',  ( 150.0000000000000000, 8.000000000000000000, 3.000000000000000000 ) ) ;
#3310 = CARTESIAN_POINT ( 'NONE',  ( 0.000000000000000000, 0.000000000000000000, -1.886264737416298631 ) ) ;
#3311 = ORIENTED_EDGE ( 'NONE', *, *, #2165, .T. ) ;
#3312 = CARTESIAN_POINT ( 'NONE',  ( -61.99999999999998579, 12.31249999999999822, 0.5000000000000013323 ) ) ;
#3313 = EDGE_CURVE ( 'NONE', #4238, #6626, #742, .T. ) ;
#3314 = ORIENTED_EDGE ( 'NONE', *, *, #4504, .F. ) ;
#3315 = CARTESIAN_POINT ( 'NONE',  ( -62.99999999999998579, 11.64583333333333748, 2.077350269189627952 ) ) ;
#3316 = AXIS2_PLACEMENT_3D ( 'NONE', #2265, #5863, #5648 ) ;
#3317 = ORIENTED_EDGE ( 'NONE', *, *, #1955, .T. ) ;
#3318 = CARTESIAN_POINT ( 'NONE',  ( -62.43234176562498305, 8.473958332991934128, 0.7511620957034662593 ) ) ;
#3319 = PLANE ( 'NONE',  #10244 ) ;
#3320 = CARTESIAN_POINT ( 'NONE',  ( -61.56765823437498852, 13.09895833299193413, 2.248837904296538515 ) ) ;
#3321 = DIRECTION ( 'NONE',  ( 0.000000000000000000, 0.000000000000000000, 1.000000000000000000 ) ) ;
#3322 = ORIENTED_EDGE ( 'NONE', *, *, #4397, .T. ) ;
#3323 = CARTESIAN_POINT ( 'NONE',  ( -61.73205080756886076, 11.02008544963257108, 0.5000000000000014433 ) ) ;
#3324 = VECTOR ( 'NONE', #6525, 1000.000000000000000 ) ;
#3325 = ORIENTED_EDGE ( 'NONE', *, *, #4423, .T. ) ;
#3326 = CARTESIAN_POINT ( 'NONE',  ( -60.99999999999998579, 12.72916666666666607, 2.077350269189628840 ) ) ;
#3327 = CARTESIAN_POINT ( 'NONE',  ( -62.43234176562498305, 15.41145833299193590, 0.7511620957034662593 ) ) ;
#3328 = DIRECTION ( 'NONE',  ( 0.000000000000000000, -1.000000000000000000, 0.000000000000000000 ) ) ;
#3329 = CARTESIAN_POINT ( 'NONE',  ( -61.99999999999999289, 12.95312499965860020, 0.5015494609379544944 ) ) ;
#3330 = CARTESIAN_POINT ( 'NONE',  ( -62.43234176562499016, 15.55729166632526628, 2.248837904296538071 ) ) ;
#3331 = CARTESIAN_POINT ( 'NONE',  ( -61.73205080756885366, 9.301335450315368902, 0.5000000000000028866 ) ) ;
#3332 = DIRECTION ( 'NONE',  ( -0.000000000000000000, -1.000000000000000000, -0.000000000000000000 ) ) ;
#3333 = ADVANCED_FACE ( 'NONE', ( #6435 ), #7316, .F. ) ;
#3334 = CARTESIAN_POINT ( 'NONE',  ( -62.43234176562498305, 8.723958332991934128, 0.7511620957034662593 ) ) ;
#3335 = CIRCLE ( 'NONE', #520, 1.000000000000000000 ) ;
#3336 = DIRECTION ( 'NONE',  ( 0.000000000000000000, 0.000000000000000000, 1.000000000000000000 ) ) ;
#3337 = ORIENTED_EDGE ( 'NONE', *, *, #3473, .T. ) ;
#3338 = CARTESIAN_POINT ( 'NONE',  ( 0.000000000000000000, 0.000000000000000000, 3.000000000000000000 ) ) ;
#3339 = CARTESIAN_POINT ( 'NONE',  ( 0.3608130681495587133, 0.2499999999999998890, -1.888070236890894815 ) ) ;
#3340 = CIRCLE ( 'NONE', #7605, 1.928074011315806136 ) ;
#3341 = CARTESIAN_POINT ( 'NONE',  ( -62.86468353124998032, 13.68229166632526805, 1.000774730468978024 ) ) ;
#3342 = CARTESIAN_POINT ( 'NONE',  ( -62.86468353124998032, 11.68229166632526805, 1.000774730468978246 ) ) ;
#3343 = CARTESIAN_POINT ( 'NONE',  ( -61.56765823437498852, 15.84895833299193590, 2.248837904296538515 ) ) ;
#3344 = VECTOR ( 'NONE', #5947, 1000.000000000000000 ) ;
#3345 = CARTESIAN_POINT ( 'NONE',  ( -61.99999999999998579, 13.18750000000000000, 2.500000000000002665 ) ) ;
#3346 = EDGE_LOOP ( 'NONE', ( #8949, #6351, #6657, #9985 ) ) ;
#3347 = CARTESIAN_POINT ( 'NONE',  ( -62.99999999999998579, 15.14583333333333215, 2.077350269189627952 ) ) ;
#3348 = CARTESIAN_POINT ( 'NONE',  ( -62.43234176562498305, 8.223958332991934128, 0.7511620957034662593 ) ) ;
#3349 =( NAMED_UNIT ( * ) PLANE_ANGLE_UNIT ( ) SI_UNIT ( $, .RADIAN. ) );
#3350 = CARTESIAN_POINT ( 'NONE',  ( -61.99999999999998579, 13.53124999931720218, 0.3452994616207497591 ) ) ;
#3351 = ORIENTED_EDGE ( 'NONE', *, *, #1326, .F. ) ;
#3352 = DIRECTION ( 'NONE',  ( 0.000000000000000000, 0.000000000000000000, 1.000000000000000000 ) ) ;
#3353 = CIRCLE ( 'NONE', #10258, 1.000000000000000888 ) ;
#3354 = CARTESIAN_POINT ( 'NONE',  ( -62.86468353124998032, 14.18229166632526983, 1.000774730468978246 ) ) ;
#3355 = CYLINDRICAL_SURFACE ( 'NONE', #6885, 1.000000000000000888 ) ;
#3356 = VERTEX_POINT ( 'NONE', #5749 ) ;
#3357 = DIRECTION ( 'NONE',  ( 1.000000000000000000, 0.000000000000000000, 0.000000000000000000 ) ) ;
#3358 = ADVANCED_FACE ( 'NONE', ( #9036 ), #9143, .T. ) ;
#3359 = COLOUR_RGB ( '',1.000000000000000000, 0.9490196078431372140, 0.9098039215686274384 ) ;
#3360 = CARTESIAN_POINT ( 'NONE',  ( -61.56765823437498142, 12.68229166632526805, 0.7511620957034663704 ) ) ;
#3361 =( BOUNDED_CURVE ( )  B_SPLINE_CURVE ( 2, ( #7632, #10343, #17, #4387, #4451, #3622, #6013, #9400, #7017 ),
 .UNSPECIFIED., .F., .T. ) 
 B_SPLINE_CURVE_WITH_KNOTS ( ( 3, 2, 2, 2, 3 ),
 ( 0.1796875000000000555, 0.1822916666666666574, 0.1875000000000000000, 0.1927083333333333426, 0.1953124999999999445 ),
 .UNSPECIFIED. ) 
 CURVE ( )  GEOMETRIC_REPRESENTATION_ITEM ( )  RATIONAL_B_SPLINE_CURVE ( ( 0.9330127018922192983, 0.9330127018922207416, 1.000000000000000000, 0.8660254037844387076, 1.000000000000000000, 0.8660254037844387076, 1.000000000000000000, 0.9330127018922207416, 0.9330127018922192983 ) ) 
 REPRESENTATION_ITEM ( '' )  );
#3362 = CARTESIAN_POINT ( 'NONE',  ( 1.299999999999999156, 0.000000000000000000, -2.000000000000000000 ) ) ;
#3363 = VERTEX_POINT ( 'NONE', #1531 ) ;
#3364 = AXIS2_PLACEMENT_3D ( 'NONE', #9053, #1441, #5707 ) ;
#3365 = DIRECTION ( 'NONE',  ( 1.000000000000000000, 0.000000000000000000, 0.000000000000000000 ) ) ;
#3366 = VERTEX_POINT ( 'NONE', #4907 ) ;
#3367 = CARTESIAN_POINT ( 'NONE',  ( -61.73205080756886076, 14.69866454968463110, 2.500000000000003109 ) ) ;
#3368 = EDGE_LOOP ( 'NONE', ( #7000, #1759, #7052, #8881 ) ) ;
#3369 = CARTESIAN_POINT ( 'NONE',  ( -62.99999999999998579, 11.60416666666666785, 0.9226497308103756012 ) ) ;
#3370 = ORIENTED_EDGE ( 'NONE', *, *, #3130, .T. ) ;
#3371 = CARTESIAN_POINT ( 'NONE',  ( -61.13531646874998415, 9.369791666325268054, 1.999225269531026417 ) ) ;
#3372 = CARTESIAN_POINT ( 'NONE',  ( -61.73205080756886076, 10.41741454900183328, 2.500000000000003109 ) ) ;
#3373 = ADVANCED_FACE ( 'NONE', ( #696 ), #9810, .T. ) ;
#3374 = CARTESIAN_POINT ( 'NONE',  ( -62.86468353124998032, 13.24479166632526983, 1.000774730468978246 ) ) ;
#3375 = DIRECTION ( 'NONE',  ( -0.000000000000000000, -0.000000000000000000, -1.000000000000000000 ) ) ;
#3376 = ORIENTED_EDGE ( 'NONE', *, *, #5610, .F. ) ;
#3377 = FACE_OUTER_BOUND ( 'NONE', #9807, .T. ) ;
#3378 = EDGE_LOOP ( 'NONE', ( #6303, #2085, #4168, #1806 ) ) ;
#3379 = PLANE ( 'NONE',  #1642 ) ;
#3380 = CARTESIAN_POINT ( 'NONE',  ( -61.56765823437498852, 15.03645833299193590, 2.248837904296538515 ) ) ;
#3381 = DIRECTION ( 'NONE',  ( 0.000000000000000000, -0.000000000000000000, -1.000000000000000000 ) ) ;
#3382 = DIRECTION ( 'NONE',  ( 0.000000000000000000, 1.000000000000000000, 0.000000000000000000 ) ) ;
#3383 = CARTESIAN_POINT ( 'NONE',  ( -61.99999999999999289, 12.07812499965860198, 2.498450539062049724 ) ) ;
#3384 = CARTESIAN_POINT ( 'NONE',  ( -62.43234176562499016, 9.494791666325268054, 2.248837904296538071 ) ) ;
#3385 = LINE ( 'NONE', #9388, #8161 ) ;
#3386 = LINE ( 'NONE', #3496, #3889 ) ;
#3387 = AXIS2_PLACEMENT_3D ( 'NONE', #6862, #1140, #5290 ) ;
#3388 = CARTESIAN_POINT ( 'NONE',  ( -61.99999999999998579, 9.578124999658601979, 2.498450539062049724 ) ) ;
#3389 = CYLINDRICAL_SURFACE ( 'NONE', #8028, 0.9999999999999981126 ) ;
#3390 = ORIENTED_EDGE ( 'NONE', *, *, #3571, .F. ) ;
#3391 = CARTESIAN_POINT ( 'NONE',  ( -61.99999999999998579, 8.656249999317202182, 2.500000000000002665 ) ) ;
#3392 = CYLINDRICAL_SURFACE ( 'NONE', #6453, 25.99999999999999645 ) ;
#3393 = CARTESIAN_POINT ( 'NONE',  ( -61.99999999999998579, 11.26562499965860198, 2.498450539062049724 ) ) ;
#3394 = CARTESIAN_POINT ( 'NONE',  ( -62.86468353124998032, 15.99479166632526628, 1.000774730468978024 ) ) ;
#3395 = CARTESIAN_POINT ( 'NONE',  ( 0.5000000000000000000, 0.2499999999999982792, 2.000000000000001776 ) ) ;
#3396 = ORIENTED_EDGE ( 'NONE', *, *, #1100, .T. ) ;
#3397 = CARTESIAN_POINT ( 'NONE',  ( -62.49999999999998579, 15.41666666666666607, 2.366025403784441483 ) ) ;
#3398 = CARTESIAN_POINT ( 'NONE',  ( -62.86468353124999453, 8.515624999658601979, 1.500000000000002220 ) ) ;
#3399 = DIRECTION ( 'NONE',  ( 1.000000000000000000, 0.000000000000000000, 0.000000000000000000 ) ) ;
#3400 = CARTESIAN_POINT ( 'NONE',  ( -61.49999999999998579, 13.92708333265053611, 2.366025403784441927 ) ) ;
#3401 = CARTESIAN_POINT ( 'NONE',  ( -62.99999999999998579, 13.10416666666666607, 0.9226497308103756012 ) ) ;
#3402 = ORIENTED_EDGE ( 'NONE', *, *, #2661, .F. ) ;
#3403 = EDGE_CURVE ( 'NONE', #3446, #470, #6124, .T. ) ;
#3404 = CIRCLE ( 'NONE', #4651, 1.934182851860892116 ) ;
#3405 = AXIS2_PLACEMENT_3D ( 'NONE', #3007, #6396, #8174 ) ;
#3406 = DIRECTION ( 'NONE',  ( -0.000000000000000000, -1.000000000000000000, -0.000000000000000000 ) ) ;
#3407 = CARTESIAN_POINT ( 'NONE',  ( -61.13531646874997705, 11.55729166632526628, 1.999225269531026417 ) ) ;
#3408 = EDGE_CURVE ( 'NONE', #607, #9265, #10677, .T. ) ;
#3409 = CARTESIAN_POINT ( 'NONE',  ( 140.0000000000000284, -8.000000000000000000, 3.000000000000000000 ) ) ;
#3410 = VERTEX_POINT ( 'NONE', #6958 ) ;
#3411 = PRESENTATION_LAYER_ASSIGNMENT (  '', '', ( #7331 ) ) ;
#3412 = CARTESIAN_POINT ( 'NONE',  ( -76.99999999999998579, 11.49999999999999645, 8.000000000000000000 ) ) ;
#3413 = VECTOR ( 'NONE', #8872, 1000.000000000000000 ) ;
#3414 = CARTESIAN_POINT ( 'NONE',  ( -61.13531646874998415, 12.89062499965860198, 1.500000000000002220 ) ) ;
#3415 = DIRECTION ( 'NONE',  ( 0.000000000000000000, 0.000000000000000000, -1.000000000000000000 ) ) ;
#3416 = ORIENTED_EDGE ( 'NONE', *, *, #7660, .T. ) ;
#3417 = PRODUCT_DEFINITION_SHAPE ( 'NONE', 'NONE',  #10983 ) ;
#3418 = DIRECTION ( 'NONE',  ( -1.000000000000000000, -0.000000000000000000, -0.000000000000000000 ) ) ;
#3419 = EDGE_LOOP ( 'NONE', ( #2541, #10410, #7823, #7330 ) ) ;
#3420 = AXIS2_PLACEMENT_3D ( 'NONE', #6348, #8910, #1403 ) ;
#3421 = DIRECTION ( 'NONE',  ( -1.000000000000000000, 0.000000000000000000, 0.000000000000000000 ) ) ;
#3422 = CARTESIAN_POINT ( 'NONE',  ( -61.13531646874998415, 11.30729166632526805, 1.999225269531026417 ) ) ;
#3423 =( BOUNDED_CURVE ( )  B_SPLINE_CURVE ( 2, ( #9013, #1406, #4784, #8189, #575, #6782, #4314, #102, #778 ),
 .UNSPECIFIED., .F., .T. ) 
 B_SPLINE_CURVE_WITH_KNOTS ( ( 3, 2, 2, 2, 3 ),
 ( 0.7421875000000000000, 0.7447916666666666297, 0.7500000000000000000, 0.7552083333333333703, 0.7578125000000000000 ),
 .UNSPECIFIED. ) 
 CURVE ( )  GEOMETRIC_REPRESENTATION_ITEM ( )  RATIONAL_B_SPLINE_CURVE ( ( 0.9330127018922194093, 0.9330127018922194093, 1.000000000000000000, 0.8660254037844387076, 1.000000000000000000, 0.8660254037844387076, 1.000000000000000000, 0.9330127018922194093, 0.9330127018922194093 ) ) 
 REPRESENTATION_ITEM ( '' )  );
#3424 = ORIENTED_EDGE ( 'NONE', *, *, #4417, .T. ) ;
#3425 = CARTESIAN_POINT ( 'NONE',  ( -62.86468353124998032, 8.994791666325268054, 1.000774730468978246 ) ) ;
#3426 = CARTESIAN_POINT ( 'NONE',  ( -61.99999999999998579, 13.78124999931720218, 0.5000000000000013323 ) ) ;
#3427 = AXIS2_PLACEMENT_3D ( 'NONE', #5834, #8445, #10785 ) ;
#3428 = EDGE_CURVE ( 'NONE', #9081, #4762, #10340, .T. ) ;
#3429 = CARTESIAN_POINT ( 'NONE',  ( -61.56765823437498142, 13.18229166632526805, 0.7511620957034663704 ) ) ;
#3430 = DIRECTION ( 'NONE',  ( 1.000000000000000000, 0.000000000000000000, 0.000000000000000000 ) ) ;
#3431 = VERTEX_POINT ( 'NONE', #9295 ) ;
#3432 = CARTESIAN_POINT ( 'NONE',  ( -60.99999999999998579, 10.98958333265053611, 0.9226497308103762673 ) ) ;
#3433 = EDGE_CURVE ( 'NONE', #9779, #869, #4977, .T. ) ;
#3434 = EDGE_LOOP ( 'NONE', ( #798, #10069, #3716, #5140 ) ) ;
#3435 = CARTESIAN_POINT ( 'NONE',  ( -62.99999999999998579, 11.61458333265053611, 2.077350269189627952 ) ) ;
#3436 = CARTESIAN_POINT ( 'NONE',  ( -61.13531646874998415, 15.84895833299193413, 1.000774730468978468 ) ) ;
#3437 = CARTESIAN_POINT ( 'NONE',  ( -61.99999999999998579, 16.03124999931720041, 0.5000000000000013323 ) ) ;
#3438 = CARTESIAN_POINT ( 'NONE',  ( -61.73205080756886076, 12.52008544963257464, 0.5000000000000014433 ) ) ;
#3439 = CARTESIAN_POINT ( 'NONE',  ( -57.99999999999998579, -14.00000000000001243, 3.000000000000000000 ) ) ;
#3440 = CARTESIAN_POINT ( 'NONE',  ( -62.86468353124998032, 12.49479166632526628, 1.000774730468978024 ) ) ;
#3441 = CARTESIAN_POINT ( 'NONE',  ( -61.56765823437498852, 8.286458332991934128, 2.248837904296538515 ) ) ;
#3442 = CARTESIAN_POINT ( 'NONE',  ( -60.99999999999998579, 9.229166666666667851, 2.077350269189628840 ) ) ;
#3443 = DIRECTION ( 'NONE',  ( -0.000000000000000000, -0.000000000000000000, 1.000000000000000000 ) ) ;
#3444 = CARTESIAN_POINT ( 'NONE',  ( -62.86468353124998032, 9.744791666325268054, 1.000774730468978246 ) ) ;
#3445 = CYLINDRICAL_SURFACE ( 'NONE', #8211, 0.9999999999999981126 ) ;
#3446 = VERTEX_POINT ( 'NONE', #348 ) ;
#3447 = CARTESIAN_POINT ( 'NONE',  ( -61.13531646874998415, 16.10937499965860198, 1.500000000000002220 ) ) ;
#3448 = CYLINDRICAL_SURFACE ( 'NONE', #2189, 1.000000000000000888 ) ;
#3449 = CARTESIAN_POINT ( 'NONE',  ( -61.13531646874998415, 15.32812499965860020, 1.500000000000002220 ) ) ;
#3450 = EDGE_CURVE ( 'NONE', #5765, #5990, #2710, .T. ) ;
#3451 = CARTESIAN_POINT ( 'NONE',  ( -62.43234176562498305, 10.66145833299193413, 0.7511620957034662593 ) ) ;
#3452 = CARTESIAN_POINT ( 'NONE',  ( -61.56765823437498142, 15.93229166632526628, 0.7511620957034663704 ) ) ;
#3453 = FACE_OUTER_BOUND ( 'NONE', #2497, .T. ) ;
#3454 = ORIENTED_EDGE ( 'NONE', *, *, #722, .T. ) ;
#3455 = CARTESIAN_POINT ( 'NONE',  ( -60.99999999999998579, 15.00000000000000000, 1.500000000000002220 ) ) ;
#3456 = CARTESIAN_POINT ( 'NONE',  ( -62.43234176562499016, 8.307291666325268054, 2.248837904296538071 ) ) ;
#3457 =( BOUNDED_CURVE ( )  B_SPLINE_CURVE ( 2, ( #5703, #3935, #4706, #8994, #653, #9989, #6554, #10597, #9153 ),
 .UNSPECIFIED., .F., .F. ) 
 B_SPLINE_CURVE_WITH_KNOTS ( ( 3, 2, 2, 2, 3 ),
 ( 0.4921875000000000000, 0.4947916666666666852, 0.5000000000000000000, 0.5052083333333333703, 0.5078125000000000000 ),
 .UNSPECIFIED. ) 
 CURVE ( )  GEOMETRIC_REPRESENTATION_ITEM ( )  RATIONAL_B_SPLINE_CURVE ( ( 0.9330127018922194093, 0.9330127018922194093, 1.000000000000000000, 0.8660254037844387076, 1.000000000000000000, 0.8660254037844387076, 1.000000000000000000, 0.9330127018922194093, 0.9330127018922194093 ) ) 
 REPRESENTATION_ITEM ( '' )  );
#3458 = CARTESIAN_POINT ( 'NONE',  ( 0.000000000000000000, 0.000000000000000000, 0.000000000000000000 ) ) ;
#3459 = CARTESIAN_POINT ( 'NONE',  ( -62.99999999999998579, 13.34374999931720396, 1.500000000000001998 ) ) ;
#3460 = FACE_OUTER_BOUND ( 'NONE', #7210, .T. ) ;
#3461 = CARTESIAN_POINT ( 'NONE',  ( -61.99999999999998579, 9.312500000000000000, 0.5000000000000013323 ) ) ;
#3462 = CARTESIAN_POINT ( 'NONE',  ( -61.13531646874997705, 11.59895833299193590, 1.000774730468978468 ) ) ;
#3463 = DIRECTION ( 'NONE',  ( 1.000000000000000000, 0.000000000000000000, 0.000000000000000000 ) ) ;
#3464 = EDGE_CURVE ( 'NONE', #10295, #7075, #8798, .T. ) ;
#3465 = CARTESIAN_POINT ( 'NONE',  ( -62.99999999999998579, 8.354166666666666075, 0.9226497308103756012 ) ) ;
#3466 = ORIENTED_EDGE ( 'NONE', *, *, #10336, .T. ) ;
#3467 = LINE ( 'NONE', #5712, #9830 ) ;
#3468 = CARTESIAN_POINT ( 'NONE',  ( -62.86468353124999453, 13.26562499965860198, 1.500000000000002220 ) ) ;
#3469 =( LENGTH_UNIT ( ) NAMED_UNIT ( * ) SI_UNIT ( .MILLI., .METRE. ) );
#3470 = CARTESIAN_POINT ( 'NONE',  ( -60.99999999999998579, 11.44791666598387003, 2.077350269189628840 ) ) ;
#3471 = CARTESIAN_POINT ( 'NONE',  ( -62.99999999999998579, 8.822916665983868256, 0.9226497308103756012 ) ) ;
#3472 = EDGE_LOOP ( 'NONE', ( #10356, #8391, #1913 ) ) ;
#3473 = EDGE_CURVE ( 'NONE', #2734, #7921, #9567, .T. ) ;
#3474 = DIRECTION ( 'NONE',  ( -1.000000000000000000, -0.000000000000000000, -0.000000000000000000 ) ) ;
#3475 = VERTEX_POINT ( 'NONE', #10622 ) ;
#3476 = CARTESIAN_POINT ( 'NONE',  ( -61.99999999999998579, 14.81250000000000000, 0.5000000000000013323 ) ) ;
#3477 = CARTESIAN_POINT ( 'NONE',  ( -62.43234176562499016, 11.24479166632526805, 2.248837904296538071 ) ) ;
#3478 = VERTEX_POINT ( 'NONE', #1180 ) ;
#3479 = CARTESIAN_POINT ( 'NONE',  ( -61.99999999999998579, 8.328124999658601979, 2.498450539062049724 ) ) ;
#3480 = CARTESIAN_POINT ( 'NONE',  ( -62.99999999999998579, 15.87500000000000000, 1.500000000000001998 ) ) ;
#3481 = CONTEXT_DEPENDENT_SHAPE_REPRESENTATION ( #8976, #1741 ) ;
#3482 = CARTESIAN_POINT ( 'NONE',  ( -61.56765823437498852, 13.34895833299193413, 2.248837904296538515 ) ) ;
#3483 = CARTESIAN_POINT ( 'NONE',  ( -62.49999999999998579, 9.385416665983870033, 2.366025403784441483 ) ) ;
#3484 = ORIENTED_EDGE ( 'NONE', *, *, #5576, .F. ) ;
#3485 = CARTESIAN_POINT ( 'NONE',  ( -53.99999999999999289, 2.939152317953647106E-15, 13.00000000000000178 ) ) ;
#3486 = ORIENTED_EDGE ( 'NONE', *, *, #8180, .T. ) ;
#3487 = CARTESIAN_POINT ( 'NONE',  ( -60.99999999999998579, 12.77083333333333393, 0.9226497308103762673 ) ) ;
#3488 = CARTESIAN_POINT ( 'NONE',  ( -61.13531646874998415, 15.34895833299193590, 1.000774730468978468 ) ) ;
#3489 = CYLINDRICAL_SURFACE ( 'NONE', #7347, 0.9999999999999981126 ) ;
#3490 = CARTESIAN_POINT ( 'NONE',  ( -60.99999999999998579, 8.218749999317202182, 1.500000000000002220 ) ) ;
#3491 = DIRECTION ( 'NONE',  ( 0.000000000000000000, 1.000000000000000000, 0.000000000000000000 ) ) ;
#3492 = CARTESIAN_POINT ( 'NONE',  ( -62.43234176562499016, 14.05729166632526805, 2.248837904296538071 ) ) ;
#3493 = CARTESIAN_POINT ( 'NONE',  ( -61.13531646874998415, 9.078124999658601979, 1.500000000000002220 ) ) ;
#3494 = EDGE_CURVE ( 'NONE', #3891, #381, #7276, .T. ) ;
#3495 = LINE ( 'NONE', #8616, #6560 ) ;
#3496 = CARTESIAN_POINT ( 'NONE',  ( -44.00000000000000000, -14.00000000000000888, 5.000000000000000000 ) ) ;
#3497 = VECTOR ( 'NONE', #7882, 1000.000000000000000 ) ;
#3498 = CARTESIAN_POINT ( 'NONE',  ( -62.86468353124999453, 9.265624999658600203, 1.500000000000002220 ) ) ;
#3499 = DIRECTION ( 'NONE',  ( -0.000000000000000000, -1.000000000000000000, -0.000000000000000000 ) ) ;
#3500 = ORIENTED_EDGE ( 'NONE', *, *, #8212, .F. ) ;
#3501 = CARTESIAN_POINT ( 'NONE',  ( -120.0000000000000000, 8.000000000000000000, 83.15773105863907233 ) ) ;
#3502 = DIRECTION ( 'NONE',  ( 0.000000000000000000, 0.000000000000000000, -1.000000000000000000 ) ) ;
#3503 = CARTESIAN_POINT ( 'NONE',  ( -62.86468353124999453, 15.20312499965860020, 1.500000000000002220 ) ) ;
#3504 = CARTESIAN_POINT ( 'NONE',  ( -61.56765823437498852, 11.03645833299193590, 2.248837904296538515 ) ) ;
#3505 = AXIS2_PLACEMENT_3D ( 'NONE', #5175, #5124, #2751 ) ;
#3506 = CARTESIAN_POINT ( 'NONE',  ( -61.13531646874997705, 8.848958332991934128, 1.000774730468978468 ) ) ;
#3507 =( NAMED_UNIT ( * ) SI_UNIT ( $, .STERADIAN. ) SOLID_ANGLE_UNIT ( ) );
#3508 = ORIENTED_EDGE ( 'NONE', *, *, #1955, .F. ) ;
#3509 = CARTESIAN_POINT ( 'NONE',  ( -62.99999999999998579, 14.87500000000000000, 1.500000000000001998 ) ) ;
#3510 = PRODUCT ( 'MAS-164', 'MAS-164', '', ( #8749 ) ) ;
#3511 = CARTESIAN_POINT ( 'NONE',  ( -62.43234176562498305, 9.723958332991934128, 0.7511620957034662593 ) ) ;
#3512 = DIRECTION ( 'NONE',  ( 0.000000000000000000, 0.000000000000000000, 1.000000000000000000 ) ) ;
#3513 = CARTESIAN_POINT ( 'NONE',  ( -62.99999999999998579, 13.09374999931720396, 1.500000000000001998 ) ) ;
#3514 = CARTESIAN_POINT ( 'NONE',  ( 0.5000000000000000000, 0.000000000000000000, 0.000000000000000000 ) ) ;
#3515 = ORIENTED_EDGE ( 'NONE', *, *, #1495, .T. ) ;
#3516 = EDGE_CURVE ( 'NONE', #5370, #8255, #2308, .T. ) ;
#3517 = CARTESIAN_POINT ( 'NONE',  ( -61.99999999999998579, 16.00000000000000000, 1.500000000000002220 ) ) ;
#3518 = AXIS2_PLACEMENT_3D ( 'NONE', #8801, #469, #10626 ) ;
#3519 = AXIS2_PLACEMENT_3D ( 'NONE', #834, #6792, #2506 ) ;
#3520 = CARTESIAN_POINT ( 'NONE',  ( -62.43234176562499016, 10.99479166632526805, 2.248837904296538071 ) ) ;
#3521 = CARTESIAN_POINT ( 'NONE',  ( -62.49999999999998579, 15.58333333333333393, 0.6339745962155627357 ) ) ;
#3522 = CARTESIAN_POINT ( 'NONE',  ( -60.99999999999998579, 13.02083333333333215, 0.9226497308103762673 ) ) ;
#3523 = ORIENTED_EDGE ( 'NONE', *, *, #9098, .T. ) ;
#3524 = PLANE ( 'NONE',  #8061 ) ;
#3525 = AXIS2_PLACEMENT_3D ( 'NONE', #8671, #8790, #10444 ) ;
#3526 = CARTESIAN_POINT ( 'NONE',  ( -62.86468353124998742, 12.53645833299193590, 1.999225269531025972 ) ) ;
#3527 = DIRECTION ( 'NONE',  ( -0.000000000000000000, -0.000000000000000000, -1.000000000000000000 ) ) ;
#3528 = CARTESIAN_POINT ( 'NONE',  ( -62.49999999999998579, 9.052083332650536107, 0.6339745962155627357 ) ) ;
#3529 = ORIENTED_EDGE ( 'NONE', *, *, #2224, .T. ) ;
#3530 = CARTESIAN_POINT ( 'NONE',  ( -103.9999999999999858, 0.000000000000000000, 13.00000000000000178 ) ) ;
#3531 = CIRCLE ( 'NONE', #10263, 1.000000000000000888 ) ;
#3532 = CARTESIAN_POINT ( 'NONE',  ( -62.43234176562498305, 11.41145833299193590, 0.7511620957034662593 ) ) ;
#3533 = SURFACE_SIDE_STYLE ('',( #6096 ) ) ;
#3534 = COLOUR_RGB ( '',0.8941176470588234615, 0.8941176470588234615, 0.8941176470588234615 ) ;
#3535 = EDGE_LOOP ( 'NONE', ( #7254, #4443, #5739, #2946 ) ) ;
#3536 = CARTESIAN_POINT ( 'NONE',  ( -61.13531646874998415, 9.390624999658600203, 1.500000000000002220 ) ) ;
#3537 = CARTESIAN_POINT ( 'NONE',  ( -61.99999999999998579, 15.68749999999999645, 2.500000000000002665 ) ) ;
#3538 = CARTESIAN_POINT ( 'NONE',  ( -61.13531646874998415, 14.39062499965860020, 1.500000000000002220 ) ) ;
#3539 = EDGE_CURVE ( 'NONE', #1175, #9392, #3353, .T. ) ;
#3540 = CARTESIAN_POINT ( 'NONE',  ( -61.99999999999998579, 9.406249999317202182, 2.500000000000002665 ) ) ;
#3541 = ORIENTED_EDGE ( 'NONE', *, *, #10290, .F. ) ;
#3542 = LINE ( 'NONE', #1773, #9395 ) ;
#3543 = ORIENTED_EDGE ( 'NONE', *, *, #9712, .T. ) ;
#3544 = CARTESIAN_POINT ( 'NONE',  ( -62.99999999999998579, 10.89583333333333393, 2.077350269189627952 ) ) ;
#3545 = EDGE_CURVE ( 'NONE', #3952, #6912, #9532, .T. ) ;
#3546 = EDGE_CURVE ( 'NONE', #10509, #4846, #2790, .T. ) ;
#3547 = CARTESIAN_POINT ( 'NONE',  ( -61.99999999999998579, 8.187500000000001776, 2.654700538379254571 ) ) ;
#3548 = CARTESIAN_POINT ( 'NONE',  ( -61.99999999999998579, 9.937500000000000000, 2.500000000000002665 ) ) ;
#3549 = LINE ( 'NONE', #1674, #5470 ) ;
#3550 = CARTESIAN_POINT ( 'NONE',  ( -62.26794919243111082, 12.29241454900182973, 0.5000000000000013323 ) ) ;
#3551 = CARTESIAN_POINT ( 'NONE',  ( -62.43234176562498305, 13.72395833299193413, 0.7511620957034662593 ) ) ;
#3552 = CARTESIAN_POINT ( 'NONE',  ( -62.86468353124999453, 9.453124999658600203, 1.500000000000002220 ) ) ;
#3553 = FACE_OUTER_BOUND ( 'NONE', #4990, .T. ) ;
#3554 = CARTESIAN_POINT ( 'NONE',  ( 150.0000000000000000, 2.500000000000000000, 3.000000000000000000 ) ) ;
#3555 = CARTESIAN_POINT ( 'NONE',  ( -62.43234176562499016, 9.557291666325268054, 2.248837904296538071 ) ) ;
#3556 = DIRECTION ( 'NONE',  ( -0.000000000000000000, -1.000000000000000000, -0.000000000000000000 ) ) ;
#3557 = ORIENTED_EDGE ( 'NONE', *, *, #1877, .F. ) ;
#3558 = CARTESIAN_POINT ( 'NONE',  ( -114.9999999999999289, -7.999999999999998224, -2.000000000000000000 ) ) ;
#3559 = DIRECTION ( 'NONE',  ( -0.000000000000000000, -1.000000000000000000, -0.000000000000000000 ) ) ;
#3560 = CARTESIAN_POINT ( 'NONE',  ( -61.13531646874998415, 16.07812499965860198, 1.500000000000002220 ) ) ;
#3561 = CARTESIAN_POINT ( 'NONE',  ( -61.56765823437498142, 11.11979166632526805, 0.7511620957034663704 ) ) ;
#3562 = CARTESIAN_POINT ( 'NONE',  ( -62.86468353124998032, 8.932291666325268054, 1.000774730468978024 ) ) ;
#3563 = ORIENTED_EDGE ( 'NONE', *, *, #8825, .T. ) ;
#3564 = CARTESIAN_POINT ( 'NONE',  ( -60.99999999999998579, 14.75000000000000000, 1.500000000000002220 ) ) ;
#3565 = CARTESIAN_POINT ( 'NONE',  ( -62.86468353124999453, 10.51562499965860198, 1.500000000000002220 ) ) ;
#3566 = SHAPE_REPRESENTATION_RELATIONSHIP ( 'NONE' , 'NONE' ,  #2752, #10920 ) ;
#3567 = CARTESIAN_POINT ( 'NONE',  ( -62.43234176562498305, 14.91145833299193590, 0.7511620957034662593 ) ) ;
#3568 = CARTESIAN_POINT ( 'NONE',  ( -61.49999999999998579, 13.17708333265053433, 2.366025403784441927 ) ) ;
#3569 = DIRECTION ( 'NONE',  ( 1.000000000000000000, -0.000000000000000000, -0.000000000000000000 ) ) ;
#3570 = ORIENTED_EDGE ( 'NONE', *, *, #4304, .T. ) ;
#3571 = EDGE_CURVE ( 'NONE', #6912, #5370, #1878, .T. ) ;
#3572 = FILL_AREA_STYLE_COLOUR ( '', #4835 ) ;
#3573 = EDGE_CURVE ( 'NONE', #9658, #7100, #10738, .T. ) ;
#3574 = CARTESIAN_POINT ( 'NONE',  ( -61.56765823437498142, 11.36979166632526805, 0.7511620957034663704 ) ) ;
#3575 = CARTESIAN_POINT ( 'NONE',  ( -62.49999999999998579, 15.66666666666666607, 2.366025403784441483 ) ) ;
#3576 = ORIENTED_EDGE ( 'NONE', *, *, #3221, .F. ) ;
#3577 = CARTESIAN_POINT ( 'NONE',  ( -61.99999999999998579, 10.68750000000000000, 2.654700538379254571 ) ) ;
#3578 = EDGE_CURVE ( 'NONE', #7065, #8335, #753, .T. ) ;
#3579 = CARTESIAN_POINT ( 'NONE',  ( -60.99999999999997868, 15.98350424826734262, 1.091118259053310835 ) ) ;
#3580 = CARTESIAN_POINT ( 'NONE',  ( -62.86468353124999453, 14.01562499965860198, 1.500000000000002220 ) ) ;
#3581 = CARTESIAN_POINT ( 'NONE',  ( -103.9999999999999858, 0.000000000000000000, 5.000000000000000000 ) ) ;
#3582 = VECTOR ( 'NONE', #8437, 1000.000000000000000 ) ;
#3583 = AXIS2_PLACEMENT_3D ( 'NONE', #1866, #4468, #2094 ) ;
#3584 = CARTESIAN_POINT ( 'NONE',  ( -62.99999999999998579, 8.864583332650536107, 2.077350269189627952 ) ) ;
#3585 = VERTEX_POINT ( 'NONE', #1509 ) ;
#3586 = CARTESIAN_POINT ( 'NONE',  ( -61.99999999999998579, -15.00000000000001421, 1.500000000000002220 ) ) ;
#3587 = CARTESIAN_POINT ( 'NONE',  ( 195.0000000000000000, 0.000000000000000000, 4.000000000000000000 ) ) ;
#3588 = VECTOR ( 'NONE', #2412, 1000.000000000000000 ) ;
#3589 = CARTESIAN_POINT ( 'NONE',  ( -61.56765823437498852, 11.53645833299193590, 2.248837904296538515 ) ) ;
#3590 = CIRCLE ( 'NONE', #6455, 0.9999999999999983347 ) ;
#3591 = ORIENTED_EDGE ( 'NONE', *, *, #4946, .T. ) ;
#3592 = EDGE_CURVE ( 'NONE', #9418, #5520, #6577, .T. ) ;
#3593 = CARTESIAN_POINT ( 'NONE',  ( -62.43234176562498305, 9.973958332991934128, 0.7511620957034662593 ) ) ;
#3594 = CARTESIAN_POINT ( 'NONE',  ( -120.0000000000000000, 3.999999999999980904, -2.000000000000000000 ) ) ;
#3595 = CIRCLE ( 'NONE', #5912, 5.000000000000018652 ) ;
#3596 = CARTESIAN_POINT ( 'NONE',  ( -61.99999999999998579, 14.45312499965860020, 0.5015494609379544944 ) ) ;
#3597 = CARTESIAN_POINT ( 'NONE',  ( 140.0000000000000284, -8.000000000000000000, 6.000000000000000000 ) ) ;
#3598 = EDGE_LOOP ( 'NONE', ( #7092, #9956, #4864, #5844 ) ) ;
#3599 = CARTESIAN_POINT ( 'NONE',  ( 0.3612935698783896754, -0.2499999999999997224, -1.888152147991466245 ) ) ;
#3600 = ADVANCED_FACE ( 'NONE', ( #6519 ), #9171, .T. ) ;
#3601 = ORIENTED_EDGE ( 'NONE', *, *, #1718, .F. ) ;
#3602 = VECTOR ( 'NONE', #6565, 1000.000000000000000 ) ;
#3603 = CARTESIAN_POINT ( 'NONE',  ( -61.73205080756886076, 12.66741454900183150, 2.500000000000003109 ) ) ;
#3604 = CARTESIAN_POINT ( 'NONE',  ( -61.99999999999998579, 8.937500000000001776, 2.654700538379254571 ) ) ;
#3605 = CARTESIAN_POINT ( 'NONE',  ( -62.99999999999998579, 9.854166666666669627, 0.9226497308103756012 ) ) ;
#3606 = PLANE ( 'NONE',  #1220 ) ;
#3607 = EDGE_CURVE ( 'NONE', #2376, #1698, #4827, .T. ) ;
#3608 = CARTESIAN_POINT ( 'NONE',  ( -104.9999999999999147, -15.00000000000001421, 0.000000000000000000 ) ) ;
#3609 = CARTESIAN_POINT ( 'NONE',  ( -62.86468353124999453, 14.53645833299193413, 1.999225269531025750 ) ) ;
#3610 = CARTESIAN_POINT ( 'NONE',  ( -61.99999999999998579, 8.890624999658601979, 0.5015494609379544944 ) ) ;
#3611 = CARTESIAN_POINT ( 'NONE',  ( -61.73205080756886076, 11.91741454900183150, 2.500000000000003109 ) ) ;
#3612 = CARTESIAN_POINT ( 'NONE',  ( -49.99999999999998579, -10.00000000000000888, 0.000000000000000000 ) ) ;
#3613 = CARTESIAN_POINT ( 'NONE',  ( -62.43234176562498305, 10.22395833299193413, 0.7511620957034662593 ) ) ;
#3614 = CARTESIAN_POINT ( 'NONE',  ( -62.99999999999998579, 14.11458333265053611, 2.077350269189627952 ) ) ;
#3615 = VERTEX_POINT ( 'NONE', #4836 ) ;
#3616 = CARTESIAN_POINT ( 'NONE',  ( -61.99999999999998579, 14.31250000000000000, 0.5000000000000013323 ) ) ;
#3617 = EDGE_CURVE ( 'NONE', #3964, #8912, #9902, .T. ) ;
#3618 = CARTESIAN_POINT ( 'NONE',  ( -62.26794919243111082, 11.32366454968462932, 0.5000000000000013323 ) ) ;
#3619 = CARTESIAN_POINT ( 'NONE',  ( -61.99999999999998579, 15.81250000000000000, 0.5000000000000013323 ) ) ;
#3620 = CARTESIAN_POINT ( 'NONE',  ( -62.86468353124998742, 11.97395833299193590, 1.999225269531025972 ) ) ;
#3621 = CARTESIAN_POINT ( 'NONE',  ( -62.86468353124999453, 8.473958332991934128, 1.999225269531025750 ) ) ;
#3622 = CARTESIAN_POINT ( 'NONE',  ( -60.99999999999998579, 9.739583332650536107, 0.9226497308103762673 ) ) ;
#3623 = ORIENTED_EDGE ( 'NONE', *, *, #10813, .T. ) ;
#3624 = CARTESIAN_POINT ( 'NONE',  ( -62.49999999999998579, 14.08333333333333393, 0.6339745962155627357 ) ) ;
#3625 = CARTESIAN_POINT ( 'NONE',  ( -62.86468353124999453, 9.765624999658601979, 1.500000000000002220 ) ) ;
#3626 = CARTESIAN_POINT ( 'NONE',  ( 0.000000000000000000, 0.000000000000000000, 0.000000000000000000 ) ) ;
#3627 = CARTESIAN_POINT ( 'NONE',  ( -62.43234176562498305, 14.66145833299193413, 0.7511620957034662593 ) ) ;
#3628 = CARTESIAN_POINT ( 'NONE',  ( -62.49999999999998579, 14.30208333265053611, 0.6339745962155627357 ) ) ;
#3629 = FACE_OUTER_BOUND ( 'NONE', #2765, .T. ) ;
#3630 = ORIENTED_EDGE ( 'NONE', *, *, #7165, .T. ) ;
#3631 = FACE_OUTER_BOUND ( 'NONE', #3368, .T. ) ;
#3632 = CARTESIAN_POINT ( 'NONE',  ( -61.56765823437498142, 12.11979166632526628, 0.7511620957034663704 ) ) ;
#3633 = CARTESIAN_POINT ( 'NONE',  ( -61.13531646874998415, 8.557291666325268054, 1.999225269531026417 ) ) ;
#3634 = VERTEX_POINT ( 'NONE', #4108 ) ;
#3635 = CARTESIAN_POINT ( 'NONE',  ( -61.49999999999998579, 11.29166666666666607, 0.6339745962155628467 ) ) ;
#3636 = EDGE_CURVE ( 'NONE', #8097, #8205, #8243, .T. ) ;
#3637 = DIRECTION ( 'NONE',  ( -0.000000000000000000, -1.000000000000000000, -0.000000000000000000 ) ) ;
#3638 = CARTESIAN_POINT ( 'NONE',  ( -61.56765823437498852, 13.59895833299193413, 2.248837904296538515 ) ) ;
#3639 = SURFACE_STYLE_USAGE ( .BOTH. , #6203 ) ;
#3640 = CARTESIAN_POINT ( 'NONE',  ( -61.99999999999998579, 9.031249999317202182, 0.3452994616207497591 ) ) ;
#3641 = ADVANCED_FACE ( 'NONE', ( #627 ), #8743, .T. ) ;
#3642 = ORIENTED_EDGE ( 'NONE', *, *, #8401, .F. ) ;
#3643 = PLANE ( 'NONE',  #8876 ) ;
#3644 = CARTESIAN_POINT ( 'NONE',  ( -62.26794919243111082, 15.39508544963257108, 2.500000000000003109 ) ) ;
#3645 = CARTESIAN_POINT ( 'NONE',  ( -62.86468353124998032, 10.93229166632526805, 1.000774730468978246 ) ) ;
#3646 = DIRECTION ( 'NONE',  ( 0.000000000000000000, 0.000000000000000000, 1.000000000000000000 ) ) ;
#3647 = ORIENTED_EDGE ( 'NONE', *, *, #10211, .T. ) ;
#3648 = CARTESIAN_POINT ( 'NONE',  ( -61.56765823437498142, 10.18229166632526805, 0.7511620957034663704 ) ) ;
#3649 = DIRECTION ( 'NONE',  ( -1.000000000000000000, 0.000000000000000000, 0.000000000000000000 ) ) ;
#3650 = CARTESIAN_POINT ( 'NONE',  ( -62.86468353124998742, 14.53645833299193413, 1.999225269531025972 ) ) ;
#3651 = LINE ( 'NONE', #10373, #2702 ) ;
#3652 = ORIENTED_EDGE ( 'NONE', *, *, #1281, .T. ) ;
#3653 =( BOUNDED_CURVE ( )  B_SPLINE_CURVE ( 2, ( #7341, #8076, #9789, #3065, #2179, #4045, #8234, #7449, #5716 ),
 .UNSPECIFIED., .F., .T. ) 
 B_SPLINE_CURVE_WITH_KNOTS ( ( 3, 2, 2, 2, 3 ),
 ( 0.8984375000000000000, 0.9010416666666666297, 0.9062500000000000000, 0.9114583333333333703, 0.9140625000000000000 ),
 .UNSPECIFIED. ) 
 CURVE ( )  GEOMETRIC_REPRESENTATION_ITEM ( )  RATIONAL_B_SPLINE_CURVE ( ( 0.9330127018922194093, 0.9330127018922194093, 1.000000000000000000, 0.8660254037844387076, 1.000000000000000000, 0.8660254037844387076, 1.000000000000000000, 0.9330127018922194093, 0.9330127018922194093 ) ) 
 REPRESENTATION_ITEM ( '' )  );
#3654 = CARTESIAN_POINT ( 'NONE',  ( -61.99999999999998579, 16.00000000000000000, 0.5000000000000041078 ) ) ;
#3655 = EDGE_CURVE ( 'NONE', #7156, #4292, #5777, .T. ) ;
#3656 = ORIENTED_EDGE ( 'NONE', *, *, #141, .F. ) ;
#3657 = CARTESIAN_POINT ( 'NONE',  ( -62.49999999999998579, 15.05208333265053611, 0.6339745962155627357 ) ) ;
#3658 = CARTESIAN_POINT ( 'NONE',  ( -61.99999999999998579, 8.812500000000000000, 0.3452994616207497591 ) ) ;
#3659 = CARTESIAN_POINT ( 'NONE',  ( -62.49999999999998579, 9.833333333333332149, 0.6339745962155627357 ) ) ;
#3660 = CARTESIAN_POINT ( 'NONE',  ( -149.9999999999999716, -8.000000000000000000, 3.000000000000000000 ) ) ;
#3661 = LINE ( 'NONE', #1227, #1568 ) ;
#3662 = CARTESIAN_POINT ( 'NONE',  ( -61.56765823437498142, 14.18229166632526805, 0.7511620957034663704 ) ) ;
#3663 = CARTESIAN_POINT ( 'NONE',  ( -61.13531646874998415, 9.828124999658601979, 1.500000000000002220 ) ) ;
#3664 =( NAMED_UNIT ( * ) PLANE_ANGLE_UNIT ( ) SI_UNIT ( $, .RADIAN. ) );
#3665 = DIRECTION ( 'NONE',  ( 0.000000000000000000, -0.000000000000000000, -1.000000000000000000 ) ) ;
#3666 = CARTESIAN_POINT ( 'NONE',  ( -61.99999999999998579, 10.57812499965860198, 2.498450539062049724 ) ) ;
#3667 = DIRECTION ( 'NONE',  ( -0.000000000000000000, -0.000000000000000000, -1.000000000000000000 ) ) ;
#3668 = ORIENTED_EDGE ( 'NONE', *, *, #1288, .F. ) ;
#3669 = FACE_OUTER_BOUND ( 'NONE', #655, .T. ) ;
#3670 = CARTESIAN_POINT ( 'NONE',  ( 145.0000000000000284, 5.500000000000000000, 6.000000000000000000 ) ) ;
#3671 = CARTESIAN_POINT ( 'NONE',  ( -62.99999999999998579, 10.36458333265053611, 2.077350269189627952 ) ) ;
#3672 = CARTESIAN_POINT ( 'NONE',  ( -61.13531646874998415, 12.82812499965860198, 1.500000000000002220 ) ) ;
#3673 = CARTESIAN_POINT ( 'NONE',  ( -61.56765823437498142, 9.119791666325268054, 0.7511620957034663704 ) ) ;
#3674 = DIRECTION ( 'NONE',  ( 0.000000000000000000, -0.000000000000000000, 1.000000000000000000 ) ) ;
#3675 = ORIENTED_EDGE ( 'NONE', *, *, #9938, .T. ) ;
#3676 = FACE_OUTER_BOUND ( 'NONE', #1957, .T. ) ;
#3677 = CARTESIAN_POINT ( 'NONE',  ( -61.13531646874998415, 10.64062499965860198, 1.500000000000002220 ) ) ;
#3678 = AXIS2_PLACEMENT_3D ( 'NONE', #439, #6441, #1331 ) ;
#3679 = DIRECTION ( 'NONE',  ( -0.1736481776669305810, 0.9848077530122082424, -5.551115123125782702E-17 ) ) ;
#3680 = CARTESIAN_POINT ( 'NONE',  ( -62.86468353124998742, 14.97395833299193590, 1.999225269531025972 ) ) ;
#3681 = CARTESIAN_POINT ( 'NONE',  ( -62.99999999999998579, 14.82291666598386826, 0.9226497308103756012 ) ) ;
#3682 = CARTESIAN_POINT ( 'NONE',  ( -62.26794919243111082, 16.14508544963257464, 2.500000000000003109 ) ) ;
#3683 = ORIENTED_EDGE ( 'NONE', *, *, #7739, .F. ) ;
#3684 = CARTESIAN_POINT ( 'NONE',  ( -164.9999999999999147, 10.63932022500206642, 3.000000000000000000 ) ) ;
#3685 = ORIENTED_EDGE ( 'NONE', *, *, #8342, .F. ) ;
#3686 =( GEOMETRIC_REPRESENTATION_CONTEXT ( 3 ) GLOBAL_UNCERTAINTY_ASSIGNED_CONTEXT ( ( #9614 ) ) GLOBAL_UNIT_ASSIGNED_CONTEXT ( ( #1804, #132, #78 ) ) REPRESENTATION_CONTEXT ( 'NONE', 'WORKASPACE' ) );
#3687 = CARTESIAN_POINT ( 'NONE',  ( -61.13531646874998415, 12.32812499965860198, 1.500000000000002220 ) ) ;
#3688 = CARTESIAN_POINT ( 'NONE',  ( -62.86468353124998742, 8.723958332991934128, 1.999225269531025972 ) ) ;
#3689 = CARTESIAN_POINT ( 'NONE',  ( -32.99999999999997158, -14.00000000000000888, 5.000000000000000000 ) ) ;
#3690 = ORIENTED_EDGE ( 'NONE', *, *, #928, .F. ) ;
#3691 = CARTESIAN_POINT ( 'NONE',  ( -62.99999999999998579, 12.39583333333333393, 2.077350269189627952 ) ) ;
#3692 = EDGE_CURVE ( 'NONE', #10524, #3634, #7507, .T. ) ;
#3693 = CARTESIAN_POINT ( 'NONE',  ( -60.99999999999998579, 8.000000000000000000, 1.500000000000002220 ) ) ;
#3694 = CARTESIAN_POINT ( 'NONE',  ( -62.43234176562498305, 13.72395833299193413, 0.7511620957034662593 ) ) ;
#3695 = SHAPE_REPRESENTATION_RELATIONSHIP ( 'NONE' , 'NONE' ,  #1195, #7741 ) ;
#3696 = AXIS2_PLACEMENT_3D ( 'NONE', #3838, #2175, #10609 ) ;
#3697 = CARTESIAN_POINT ( 'NONE',  ( -61.99999999999998579, 10.65624999931720218, 2.654700538379254571 ) ) ;
#3698 = ORIENTED_EDGE ( 'NONE', *, *, #6843, .T. ) ;
#3699 = CARTESIAN_POINT ( 'NONE',  ( -61.49999999999998579, 13.95833333333333215, 2.366025403784441927 ) ) ;
#3700 = VECTOR ( 'NONE', #6450, 1000.000000000000000 ) ;
#3701 = CARTESIAN_POINT ( 'NONE',  ( -61.99999999999998579, 10.03124999931720218, 0.5000000000000013323 ) ) ;
#3702 = CARTESIAN_POINT ( 'NONE',  ( -62.86468353124998742, 11.97395833299193590, 1.999225269531025972 ) ) ;
#3703 = CARTESIAN_POINT ( 'NONE',  ( 0.5000000000000000000, -0.2500000000000000000, 1.911797424705720116 ) ) ;
#3704 = VECTOR ( 'NONE', #9287, 1000.000000000000000 ) ;
#3705 = EDGE_CURVE ( 'NONE', #3363, #6433, #3025, .T. ) ;
#3706 = EDGE_LOOP ( 'NONE', ( #8583, #4737, #2374, #3623 ) ) ;
#3707 = CARTESIAN_POINT ( 'NONE',  ( -61.13531646874998415, 9.640624999658601979, 1.500000000000002220 ) ) ;
#3708 = DIRECTION ( 'NONE',  ( 0.000000000000000000, -1.000000000000000000, 0.000000000000000000 ) ) ;
#3709 = VECTOR ( 'NONE', #5631, 1000.000000000000000 ) ;
#3710 = CARTESIAN_POINT ( 'NONE',  ( -61.99999999999998579, 14.20312499965860198, 0.5015494609379544944 ) ) ;
#3711 = FACE_OUTER_BOUND ( 'NONE', #9027, .T. ) ;
#3712 = ORIENTED_EDGE ( 'NONE', *, *, #3145, .T. ) ;
#3713 = DIRECTION ( 'NONE',  ( -1.000000000000000000, -0.000000000000000000, -0.000000000000000000 ) ) ;
#3714 =( GEOMETRIC_REPRESENTATION_CONTEXT ( 3 ) GLOBAL_UNCERTAINTY_ASSIGNED_CONTEXT ( ( #407 ) ) GLOBAL_UNIT_ASSIGNED_CONTEXT ( ( #5246, #1090, #922 ) ) REPRESENTATION_CONTEXT ( 'NONE', 'WORKASPACE' ) );
#3715 = APPLICATION_CONTEXT ( 'automotive_design' ) ;
#3716 = ORIENTED_EDGE ( 'NONE', *, *, #5091, .T. ) ;
#3717 = CARTESIAN_POINT ( 'NONE',  ( -61.99999999999998579, 16.00000000000000000, 0.5000000000000041078 ) ) ;
#3718 = CARTESIAN_POINT ( 'NONE',  ( -60.99999999999998579, 8.750000000000000000, 1.500000000000002220 ) ) ;
#3719 = AXIS2_PLACEMENT_3D ( 'NONE', #6046, #5088, #825 ) ;
#3720 = LINE ( 'NONE', #8122, #1664 ) ;
#3721 = CARTESIAN_POINT ( 'NONE',  ( -61.49999999999998579, 16.17708333265053255, 2.366025403784441927 ) ) ;
#3722 = DIRECTION ( 'NONE',  ( 0.000000000000000000, 0.000000000000000000, 1.000000000000000000 ) ) ;
#3723 = CARTESIAN_POINT ( 'NONE',  ( -61.13531646874998415, 14.39062499965860020, 1.500000000000002220 ) ) ;
#3724 = ADVANCED_FACE ( 'NONE', ( #3173 ), #2339, .T. ) ;
#3725 = CARTESIAN_POINT ( 'NONE',  ( -62.43234176562499016, 10.24479166632526805, 2.248837904296538071 ) ) ;
#3726 =( GEOMETRIC_REPRESENTATION_CONTEXT ( 3 ) GLOBAL_UNCERTAINTY_ASSIGNED_CONTEXT ( ( #7376 ) ) GLOBAL_UNIT_ASSIGNED_CONTEXT ( ( #8986, #3096, #4859 ) ) REPRESENTATION_CONTEXT ( 'NONE', 'WORKASPACE' ) );
#3727 = DIRECTION ( 'NONE',  ( 1.000000000000000000, 0.000000000000000000, 0.000000000000000000 ) ) ;
#3728 =( BOUNDED_CURVE ( )  B_SPLINE_CURVE ( 2, ( #4510, #5396, #4453, #6245, #2796, #7913, #471, #8803, #7076 ),
 .UNSPECIFIED., .F., .F. ) 
 B_SPLINE_CURVE_WITH_KNOTS ( ( 3, 2, 2, 2, 3 ),
 ( 0.3203125000000000000, 0.3229166666666666852, 0.3281250000000000000, 0.3333333333333333148, 0.3359374999999999445 ),
 .UNSPECIFIED. ) 
 CURVE ( )  GEOMETRIC_REPRESENTATION_ITEM ( )  RATIONAL_B_SPLINE_CURVE ( ( 0.9330127018922194093, 0.9330127018922194093, 1.000000000000000000, 0.8660254037844387076, 1.000000000000000000, 0.8660254037844387076, 1.000000000000000000, 0.9330127018922207416, 0.9330127018922192983 ) ) 
 REPRESENTATION_ITEM ( '' )  );
#3729 = LINE ( 'NONE', #1172, #10253 ) ;
#3730 = CARTESIAN_POINT ( 'NONE',  ( -61.56765823437498852, 10.34895833299193413, 2.248837904296538515 ) ) ;
#3731 = PLANE ( 'NONE',  #752 ) ;
#3732 = ORIENTED_EDGE ( 'NONE', *, *, #7187, .T. ) ;
#3733 = CARTESIAN_POINT ( 'NONE',  ( -77.99999999999998579, 11.49999999999999645, 5.000000000000000000 ) ) ;
#3734 = CARTESIAN_POINT ( 'NONE',  ( -101.9999999999999858, 0.000000000000000000, 13.00000000000000178 ) ) ;
#3735 = EDGE_LOOP ( 'NONE', ( #10063, #3849, #10923, #8656 ) ) ;
#3736 = DIRECTION ( 'NONE',  ( -0.000000000000000000, -1.000000000000000000, -0.000000000000000000 ) ) ;
#3737 = CARTESIAN_POINT ( 'NONE',  ( -62.43234176562498305, 11.91145833299193413, 0.7511620957034662593 ) ) ;
#3738 = CARTESIAN_POINT ( 'NONE',  ( -61.13531646874998415, 9.828124999658601979, 1.500000000000002220 ) ) ;
#3739 = DIRECTION ( 'NONE',  ( -1.000000000000000000, 0.000000000000000000, 0.000000000000000000 ) ) ;
#3740 = EDGE_LOOP ( 'NONE', ( #4279, #478 ) ) ;
#3741 = CARTESIAN_POINT ( 'NONE',  ( -61.49999999999998579, 8.510416665983868256, 0.6339745962155628467 ) ) ;
#3742 = CARTESIAN_POINT ( 'NONE',  ( -62.86468353124999453, 10.53645833299193413, 1.999225269531025750 ) ) ;
#3743 =( NAMED_UNIT ( * ) PLANE_ANGLE_UNIT ( ) SI_UNIT ( $, .RADIAN. ) );
#3744 = CARTESIAN_POINT ( 'NONE',  ( -61.56765823437498142, 14.86979166632526805, 0.7511620957034663704 ) ) ;
#3745 = CARTESIAN_POINT ( 'NONE',  ( -62.99999999999998579, 15.11458333265053433, 2.077350269189627952 ) ) ;
#3746 = FACE_OUTER_BOUND ( 'NONE', #615, .T. ) ;
#3747 = VERTEX_POINT ( 'NONE', #10007 ) ;
#3748 = CARTESIAN_POINT ( 'NONE',  ( -61.99999999999998579, 16.00000000000000000, 0.5000000000000041078 ) ) ;
#3749 = ORIENTED_EDGE ( 'NONE', *, *, #3428, .F. ) ;
#3750 = CARTESIAN_POINT ( 'NONE',  ( -62.86468353124999453, 12.72395833299193413, 1.999225269531025750 ) ) ;
#3751 = CARTESIAN_POINT ( 'NONE',  ( -61.13531646874998415, 8.598958332991934128, 1.000774730468978468 ) ) ;
#3752 = CARTESIAN_POINT ( 'NONE',  ( -77.99999999999998579, -11.50000000000000711, 5.000000000000000000 ) ) ;
#3753 = ORIENTED_EDGE ( 'NONE', *, *, #6750, .T. ) ;
#3754 = CARTESIAN_POINT ( 'NONE',  ( -60.99999999999998579, 12.00000000000000000, 1.500000000000002220 ) ) ;
#3755 = DIRECTION ( 'NONE',  ( 0.000000000000000000, 0.000000000000000000, -1.000000000000000000 ) ) ;
#3756 = CARTESIAN_POINT ( 'NONE',  ( -62.86468353124999453, 14.76562499965860020, 1.500000000000002220 ) ) ;
#3757 = EDGE_CURVE ( 'NONE', #6540, #7871, #670, .T. ) ;
#3758 = CARTESIAN_POINT ( 'NONE',  ( -61.99999999999998579, 16.00000000000000000, 1.500000000000002220 ) ) ;
#3759 = CARTESIAN_POINT ( 'NONE',  ( -62.49999999999998579, 10.55208333265053611, 0.6339745962155627357 ) ) ;
#3760 = ORIENTED_EDGE ( 'NONE', *, *, #10548, .T. ) ;
#3761 = VECTOR ( 'NONE', #4218, 1000.000000000000000 ) ;
#3762 = CARTESIAN_POINT ( 'NONE',  ( -105.0000000000000000, 2.500000000000000000, 3.000000000000000000 ) ) ;
#3763 = CARTESIAN_POINT ( 'NONE',  ( -61.73205080756886076, 9.917414549001833279, 2.500000000000003109 ) ) ;
#3764 = EDGE_CURVE ( 'NONE', #7557, #4954, #5831, .T. ) ;
#3765 = CARTESIAN_POINT ( 'NONE',  ( -62.86468353124999453, 12.45312499965860198, 1.500000000000002220 ) ) ;
#3766 = FILL_AREA_STYLE_COLOUR ( '', #499 ) ;
#3767 = ORIENTED_EDGE ( 'NONE', *, *, #2619, .F. ) ;
#3768 = AXIS2_PLACEMENT_3D ( 'NONE', #3597, #1098, #6158 ) ;
#3769 = CARTESIAN_POINT ( 'NONE',  ( -61.99999999999998579, 10.82812499965860198, 2.498450539062049724 ) ) ;
#3770 = CARTESIAN_POINT ( 'NONE',  ( -62.49999999999998579, 15.63541666598386826, 2.366025403784441483 ) ) ;
#3771 = CARTESIAN_POINT ( 'NONE',  ( -62.86468353124998742, 14.78645833299193413, 1.999225269531025972 ) ) ;
#3772 = DIRECTION ( 'NONE',  ( 1.000000000000000000, 0.000000000000000000, 0.000000000000000000 ) ) ;
#3773 = ORIENTED_EDGE ( 'NONE', *, *, #3573, .F. ) ;
#3774 = VECTOR ( 'NONE', #3430, 1000.000000000000000 ) ;
#3775 = DIRECTION ( 'NONE',  ( 1.000000000000000000, -0.000000000000000000, 0.000000000000000000 ) ) ;
#3776 = AXIS2_PLACEMENT_3D ( 'NONE', #5552, #6665, #9945 ) ;
#3777 = ORIENTED_EDGE ( 'NONE', *, *, #1352, .T. ) ;
#3778 = DIRECTION ( 'NONE',  ( -0.000000000000000000, -1.000000000000000000, -0.000000000000000000 ) ) ;
#3779 = CARTESIAN_POINT ( 'NONE',  ( -62.86468353124999453, 15.95312499965860198, 1.500000000000002220 ) ) ;
#3780 = FACE_OUTER_BOUND ( 'NONE', #10079, .T. ) ;
#3781 = CARTESIAN_POINT ( 'NONE',  ( -61.99999999999998579, 11.93750000000000000, 2.500000000000002665 ) ) ;
#3782 = DIRECTION ( 'NONE',  ( 0.000000000000000000, 1.000000000000000000, 0.000000000000000000 ) ) ;
#3783 = AXIS2_PLACEMENT_3D ( 'NONE', #2513, #6689, #10851 ) ;
#3784 = EDGE_CURVE ( 'NONE', #5388, #5305, #3423, .T. ) ;
#3785 = CARTESIAN_POINT ( 'NONE',  ( -62.86468353124998032, 14.74479166632526983, 1.000774730468978024 ) ) ;
#3786 = CARTESIAN_POINT ( 'NONE',  ( -61.56765823437498852, 10.28645833299193413, 2.248837904296538515 ) ) ;
#3787 = CARTESIAN_POINT ( 'NONE',  ( -62.99999999999998579, 11.34374999931720218, 1.500000000000001998 ) ) ;
#3788 = PLANE ( 'NONE',  #9928 ) ;
#3789 = CARTESIAN_POINT ( 'NONE',  ( -62.43234176562499016, 10.30729166632526983, 2.248837904296538071 ) ) ;
#3790 = EDGE_CURVE ( 'NONE', #1925, #10979, #4561, .T. ) ;
#3791 = CARTESIAN_POINT ( 'NONE',  ( -62.99999999999998579, 13.64583333333333215, 2.077350269189627952 ) ) ;
#3792 = VERTEX_POINT ( 'NONE', #4157 ) ;
#3793 = CARTESIAN_POINT ( 'NONE',  ( -61.99999999999998579, 14.43749999999999822, 2.500000000000002665 ) ) ;
#3794 = CARTESIAN_POINT ( 'NONE',  ( 1.084202172485504434E-16, 0.000000000000000000, 0.000000000000000000 ) ) ;
#3795 = VECTOR ( 'NONE', #4515, 1000.000000000000000 ) ;
#3796 = EDGE_LOOP ( 'NONE', ( #2519, #2032, #2907, #2044 ) ) ;
#3797 = CARTESIAN_POINT ( 'NONE',  ( -62.99999999999998579, 10.34374999931720218, 1.500000000000001998 ) ) ;
#3798 = CARTESIAN_POINT ( 'NONE',  ( -61.56765823437498142, 11.86979166632526805, 0.7511620957034663704 ) ) ;
#3799 = CARTESIAN_POINT ( 'NONE',  ( -62.86468353124999453, 10.72395833299193413, 1.999225269531025750 ) ) ;
#3800 = CARTESIAN_POINT ( 'NONE',  ( -62.99999999999998579, 8.604166666666666075, 0.9226497308103756012 ) ) ;
#3801 =( BOUNDED_CURVE ( )  B_SPLINE_CURVE ( 2, ( #8603, #210, #156, #4202, #982, #7772, #3483, #7607, #3540 ),
 .UNSPECIFIED., .F., .T. ) 
 B_SPLINE_CURVE_WITH_KNOTS ( ( 3, 2, 2, 2, 3 ),
 ( 0.1328125000000000000, 0.1354166666666666574, 0.1406250000000000000, 0.1458333333333333426, 0.1484374999999999722 ),
 .UNSPECIFIED. ) 
 CURVE ( )  GEOMETRIC_REPRESENTATION_ITEM ( )  RATIONAL_B_SPLINE_CURVE ( ( 0.9330127018922194093, 0.9330127018922194093, 1.000000000000000000, 0.8660254037844387076, 1.000000000000000000, 0.8660254037844387076, 1.000000000000000000, 0.9330127018922200755, 0.9330127018922194093 ) ) 
 REPRESENTATION_ITEM ( '' )  );
#3802 = VERTEX_POINT ( 'NONE', #4366 ) ;
#3803 = FACE_OUTER_BOUND ( 'NONE', #4271, .T. ) ;
#3804 = CARTESIAN_POINT ( 'NONE',  ( -62.86468353124999453, 11.01562499965860020, 1.500000000000002220 ) ) ;
#3805 = APPLICATION_PROTOCOL_DEFINITION ( 'draft international standard', 'automotive_design', 1998, #4401 ) ;
#3806 = CARTESIAN_POINT ( 'NONE',  ( -62.86468353124998032, 14.68229166632526805, 1.000774730468978246 ) ) ;
#3807 = CARTESIAN_POINT ( 'NONE',  ( -60.99999999999998579, 15.21874999931720218, 1.500000000000002220 ) ) ;
#3808 = CARTESIAN_POINT ( 'NONE',  ( 0.000000000000000000, -0.2499999999999998335, -1.312875263449798879 ) ) ;
#3809 = EDGE_LOOP ( 'NONE', ( #3826, #2795, #9159, #7912 ) ) ;
#3810 = CARTESIAN_POINT ( 'NONE',  ( -61.99999999999998579, 16.00000000000000000, 0.5000000000000041078 ) ) ;
#3811 = ORIENTED_EDGE ( 'NONE', *, *, #1647, .T. ) ;
#3812 = EDGE_CURVE ( 'NONE', #4311, #10281, #5702, .T. ) ;
#3813 = CARTESIAN_POINT ( 'NONE',  ( -61.13531646874997705, 13.30729166632526983, 1.999225269531026417 ) ) ;
#3814 = CARTESIAN_POINT ( 'NONE',  ( -61.56765823437498852, 8.286458332991934128, 2.248837904296538515 ) ) ;
#3815 = CARTESIAN_POINT ( 'NONE',  ( -61.99999999999998579, 11.68749999999999822, 2.500000000000002665 ) ) ;
#3816 = ORIENTED_EDGE ( 'NONE', *, *, #10358, .F. ) ;
#3817 = CARTESIAN_POINT ( 'NONE',  ( -62.49999999999998579, 11.83333333333333215, 0.6339745962155627357 ) ) ;
#3818 = CARTESIAN_POINT ( 'NONE',  ( -60.99999999999998579, 15.96874999931720218, 1.500000000000002220 ) ) ;
#3819 = SHAPE_REPRESENTATION_RELATIONSHIP ( 'NONE' , 'NONE' ,  #10405, #7886 ) ;
#3820 = CARTESIAN_POINT ( 'NONE',  ( -62.26794919243111082, 14.39508544963257286, 2.500000000000003109 ) ) ;
#3821 = CARTESIAN_POINT ( 'NONE',  ( -62.49999999999998579, 11.13541666598387003, 2.366025403784441483 ) ) ;
#3822 = VERTEX_POINT ( 'NONE', #7558 ) ;
#3823 = DIRECTION ( 'NONE',  ( 1.000000000000000000, 0.000000000000000000, 0.000000000000000000 ) ) ;
#3824 = EDGE_CURVE ( 'NONE', #6498, #192, #1717, .T. ) ;
#3825 = CARTESIAN_POINT ( 'NONE',  ( -61.99999999999998579, 13.01562499965860198, 2.498450539062049724 ) ) ;
#3826 = ORIENTED_EDGE ( 'NONE', *, *, #6064, .T. ) ;
#3827 = CARTESIAN_POINT ( 'NONE',  ( -61.13531646874998415, 9.911458332991935904, 1.000774730468978468 ) ) ;
#3828 = CARTESIAN_POINT ( 'NONE',  ( -62.49999999999998579, 12.55208333265053611, 0.6339745962155627357 ) ) ;
#3829 = ADVANCED_FACE ( 'NONE', ( #9325 ), #5093, .T. ) ;
#3830 = CARTESIAN_POINT ( 'NONE',  ( -62.86468353124998032, 15.49479166632526628, 1.000774730468978246 ) ) ;
#3831 = DIRECTION ( 'NONE',  ( 0.000000000000000000, -0.000000000000000000, 1.000000000000000000 ) ) ;
#3832 = ORIENTED_EDGE ( 'NONE', *, *, #928, .T. ) ;
#3833 = CARTESIAN_POINT ( 'NONE',  ( -61.49999999999998579, 10.45833333333333393, 2.366025403784441927 ) ) ;
#3834 = ORIENTED_EDGE ( 'NONE', *, *, #8863, .F. ) ;
#3835 = LINE ( 'NONE', #9550, #2353 ) ;
#3836 = CARTESIAN_POINT ( 'NONE',  ( -61.99999999999998579, 10.18750000000000000, 2.654700538379254571 ) ) ;
#3837 = CARTESIAN_POINT ( 'NONE',  ( -61.99999999999998579, 11.31250000000000000, 0.5000000000000013323 ) ) ;
#3838 = CARTESIAN_POINT ( 'NONE',  ( 0.000000000000000000, 0.000000000000000000, 4.000000000000000000 ) ) ;
#3839 = CARTESIAN_POINT ( 'NONE',  ( 1.299999999999999156, 0.000000000000000000, 0.000000000000000000 ) ) ;
#3840 = CARTESIAN_POINT ( 'NONE',  ( -61.13531646874998415, 10.30729166632526805, 1.999225269531026417 ) ) ;
#3841 = CARTESIAN_POINT ( 'NONE',  ( -62.26794919243111082, 11.29241454900183328, 0.4999999999999982792 ) ) ;
#3842 = LINE ( 'NONE', #1291, #10970 ) ;
#3843 = CARTESIAN_POINT ( 'NONE',  ( -61.56765823437498852, 10.84895833299193413, 2.248837904296538515 ) ) ;
#3844 = CARTESIAN_POINT ( 'NONE',  ( -62.99999999999998579, 12.10416666666666607, 0.9226497308103756012 ) ) ;
#3845 = EDGE_LOOP ( 'NONE', ( #4077, #858, #3142, #4779 ) ) ;
#3846 = CARTESIAN_POINT ( 'NONE',  ( -61.99999999999998579, 13.90624999931720218, 2.500000000000002665 ) ) ;
#3847 = UNCERTAINTY_MEASURE_WITH_UNIT (LENGTH_MEASURE( 1.000000000000000082E-05 ), #4408, 'distance_accuracy_value', 'NONE');
#3848 = LINE ( 'NONE', #3734, #1825 ) ;
#3849 = ORIENTED_EDGE ( 'NONE', *, *, #9213, .T. ) ;
#3850 = CARTESIAN_POINT ( 'NONE',  ( -61.49999999999998579, 10.26041666598387003, 0.6339745962155628467 ) ) ;
#3851 = CARTESIAN_POINT ( 'NONE',  ( -62.43234176562498305, 12.41145833299193413, 0.7511620957034662593 ) ) ;
#3852 = EDGE_CURVE ( 'NONE', #1800, #6871, #4143, .T. ) ;
#3853 = CARTESIAN_POINT ( 'NONE',  ( -61.13531646874998415, 9.578124999658600203, 1.500000000000002220 ) ) ;
#3854 = CARTESIAN_POINT ( 'NONE',  ( -61.99999999999998579, 12.53124999931720396, 0.5000000000000013323 ) ) ;
#3855 = ORIENTED_EDGE ( 'NONE', *, *, #6412, .T. ) ;
#3856 = CARTESIAN_POINT ( 'NONE',  ( -61.73205080756884655, 8.417414549001831503, 2.500000000000004885 ) ) ;
#3857 = CARTESIAN_POINT ( 'NONE',  ( -61.99999999999999289, 11.07812499965860020, 2.498450539062049724 ) ) ;
#3858 = DIRECTION ( 'NONE',  ( 1.000000000000000000, 0.000000000000000000, 0.000000000000000000 ) ) ;
#3859 = CARTESIAN_POINT ( 'NONE',  ( -62.49999999999998579, 13.63541666598387003, 2.366025403784441483 ) ) ;
#3860 = CARTESIAN_POINT ( 'NONE',  ( -60.99999999999998579, 14.98958333265053788, 0.9226497308103762673 ) ) ;
#3861 = CARTESIAN_POINT ( 'NONE',  ( -61.73205080756886076, 14.66741454900183150, 2.500000000000003109 ) ) ;
#3862 = ORIENTED_EDGE ( 'NONE', *, *, #8457, .F. ) ;
#3863 = DIRECTION ( 'NONE',  ( 1.000000000000000000, -0.000000000000000000, -0.000000000000000000 ) ) ;
#3864 = VERTEX_POINT ( 'NONE', #4260 ) ;
#3865 =( BOUNDED_CURVE ( )  B_SPLINE_CURVE ( 2, ( #6483, #7201, #10635, #2203, #2253, #590, #2926, #10696, #1254 ),
 .UNSPECIFIED., .F., .T. ) 
 B_SPLINE_CURVE_WITH_KNOTS ( ( 3, 2, 2, 2, 3 ),
 ( 0.8671875000000000000, 0.8697916666666666297, 0.8750000000000000000, 0.8802083333333333703, 0.8828125000000000000 ),
 .UNSPECIFIED. ) 
 CURVE ( )  GEOMETRIC_REPRESENTATION_ITEM ( )  RATIONAL_B_SPLINE_CURVE ( ( 0.9330127018922194093, 0.9330127018922194093, 1.000000000000000000, 0.8660254037844387076, 1.000000000000000000, 0.8660254037844387076, 1.000000000000000000, 0.9330127018922194093, 0.9330127018922194093 ) ) 
 REPRESENTATION_ITEM ( '' )  );
#3866 = CARTESIAN_POINT ( 'NONE',  ( -62.86468353124998032, 13.43229166632526983, 1.000774730468978024 ) ) ;
#3867 = CARTESIAN_POINT ( 'NONE',  ( -61.56765823437498852, 8.786458332991934128, 2.248837904296538515 ) ) ;
#3868 = CIRCLE ( 'NONE', #9899, 5.000000000000018652 ) ;
#3869 = CARTESIAN_POINT ( 'NONE',  ( -60.99999999999998579, 11.72916666666666785, 2.077350269189628840 ) ) ;
#3870 = ORIENTED_EDGE ( 'NONE', *, *, #5076, .T. ) ;
#3871 = CARTESIAN_POINT ( 'NONE',  ( -61.99999999999998579, 11.81250000000000000, 0.3452994616207497591 ) ) ;
#3872 = CARTESIAN_POINT ( 'NONE',  ( -62.99999999999998579, 8.593749999317203958, 1.500000000000001998 ) ) ;
#3873 = CARTESIAN_POINT ( 'NONE',  ( 150.0000000000000000, -8.000000000000000000, 3.000000000000000000 ) ) ;
#3874 = ADVANCED_FACE ( 'NONE', ( #2723 ), #3379, .F. ) ;
#3875 = CARTESIAN_POINT ( 'NONE',  ( -61.99999999999998579, 10.90624999931720218, 2.654700538379254571 ) ) ;
#3876 = ORIENTED_EDGE ( 'NONE', *, *, #7132, .T. ) ;
#3877 = VECTOR ( 'NONE', #1128, 999.9999999999998863 ) ;
#3878 = DIRECTION ( 'NONE',  ( 0.000000000000000000, 0.000000000000000000, 1.000000000000000000 ) ) ;
#3879 = CARTESIAN_POINT ( 'NONE',  ( -62.86468353124998742, 12.47395833299193413, 1.999225269531025972 ) ) ;
#3880 =( LENGTH_UNIT ( ) NAMED_UNIT ( * ) SI_UNIT ( .MILLI., .METRE. ) );
#3881 = VERTEX_POINT ( 'NONE', #5991 ) ;
#3882 = CIRCLE ( 'NONE', #8483, 1.928074011315806136 ) ;
#3883 = CARTESIAN_POINT ( 'NONE',  ( -62.86468353124999453, 11.01562499965860020, 1.500000000000002220 ) ) ;
#3884 = DIRECTION ( 'NONE',  ( -0.000000000000000000, -1.000000000000000000, -0.000000000000000000 ) ) ;
#3885 = VECTOR ( 'NONE', #2998, 1000.000000000000000 ) ;
#3886 = CARTESIAN_POINT ( 'NONE',  ( -61.99999999999998579, 16.07812499965860198, 2.498450539062049724 ) ) ;
#3887 = ORIENTED_EDGE ( 'NONE', *, *, #2925, .F. ) ;
#3888 = CARTESIAN_POINT ( 'NONE',  ( -49.99999999999998579, -10.00000000000000888, -0.1418111474832519925 ) ) ;
#3889 = VECTOR ( 'NONE', #2507, 1000.000000000000000 ) ;
#3890 = VECTOR ( 'NONE', #4949, 1000.000000000000000 ) ;
#3891 = VERTEX_POINT ( 'NONE', #1670 ) ;
#3892 = CARTESIAN_POINT ( 'NONE',  ( -61.99999999999998579, 16.00000000000000000, 0.5000000000000041078 ) ) ;
#3893 = CARTESIAN_POINT ( 'NONE',  ( -60.99999999999998579, 9.500000000000000000, 1.500000000000002220 ) ) ;
#3894 = CARTESIAN_POINT ( 'NONE',  ( -101.9999999999999858, 0.000000000000000000, 13.00000000000000178 ) ) ;
#3895 = DIRECTION ( 'NONE',  ( 0.000000000000000000, 0.000000000000000000, -1.000000000000000000 ) ) ;
#3896 =( BOUNDED_CURVE ( )  B_SPLINE_CURVE ( 2, ( #110, #4439, #59, #3442, #5264, #1679, #7787, #3331, #8670 ),
 .UNSPECIFIED., .F., .F. ) 
 B_SPLINE_CURVE_WITH_KNOTS ( ( 3, 2, 2, 2, 3 ),
 ( 0.1484374999999999722, 0.1510416666666666574, 0.1562500000000000000, 0.1614583333333333426, 0.1640624999999999722 ),
 .UNSPECIFIED. ) 
 CURVE ( )  GEOMETRIC_REPRESENTATION_ITEM ( )  RATIONAL_B_SPLINE_CURVE ( ( 0.9330127018922194093, 0.9330127018922186322, 1.000000000000000000, 0.8660254037844387076, 1.000000000000000000, 0.8660254037844387076, 1.000000000000000000, 0.9330127018922200755, 0.9330127018922194093 ) ) 
 REPRESENTATION_ITEM ( '' )  );
#3897 = CARTESIAN_POINT ( 'NONE',  ( -61.99999999999998579, 14.78124999931720218, 0.5000000000000013323 ) ) ;
#3898 = VECTOR ( 'NONE', #6147, 1000.000000000000000 ) ;
#3899 = CARTESIAN_POINT ( 'NONE',  ( -60.99999999999998579, 8.447916665983870033, 2.077350269189628840 ) ) ;
#3900 = CARTESIAN_POINT ( 'NONE',  ( -61.99999999999998579, 12.45312499965860020, 0.5015494609379544944 ) ) ;
#3901 = CARTESIAN_POINT ( 'NONE',  ( -61.99999999999998579, 14.99999999999998579, 2.500000000000003109 ) ) ;
#3902 = ORIENTED_EDGE ( 'NONE', *, *, #9235, .T. ) ;
#3903 = LINE ( 'NONE', #7294, #6212 ) ;
#3904 = PLANE ( 'NONE',  #7164 ) ;
#3905 = EDGE_CURVE ( 'NONE', #10857, #1159, #10170, .T. ) ;
#3906 = AXIS2_PLACEMENT_3D ( 'NONE', #6884, #47, #10933 ) ;
#3907 = ORIENTED_EDGE ( 'NONE', *, *, #4221, .T. ) ;
#3908 = CARTESIAN_POINT ( 'NONE',  ( -134.9999999999999147, 8.000000000000000000, 3.000000000000000000 ) ) ;
#3909 = CARTESIAN_POINT ( 'NONE',  ( -62.43234176562498305, 13.91145833299193413, 0.7511620957034662593 ) ) ;
#3910 = CARTESIAN_POINT ( 'NONE',  ( -61.56765823437498142, 10.86979166632526805, 0.7511620957034663704 ) ) ;
#3911 = EDGE_LOOP ( 'NONE', ( #7689, #2686, #343, #4233 ) ) ;
#3912 = CARTESIAN_POINT ( 'NONE',  ( -62.99999999999998579, 14.14583333333333393, 2.077350269189627952 ) ) ;
#3913 = CARTESIAN_POINT ( 'NONE',  ( -62.43234176562499016, 11.30729166632526805, 2.248837904296538071 ) ) ;
#3914 = DIRECTION ( 'NONE',  ( -0.000000000000000000, -0.000000000000000000, -1.000000000000000000 ) ) ;
#3915 = CONICAL_SURFACE ( 'NONE', #5308, 6.000000000000005329, 0.7853981633974479459 ) ;
#3916 = CARTESIAN_POINT ( 'NONE',  ( -62.99999999999998579, 15.59374999931720218, 1.500000000000001998 ) ) ;
#3917 = CARTESIAN_POINT ( 'NONE',  ( -62.99999999999998579, 16.09374999931720396, 1.500000000000001998 ) ) ;
#3918 = ORIENTED_EDGE ( 'NONE', *, *, #8577, .T. ) ;
#3919 = DIRECTION ( 'NONE',  ( 0.000000000000000000, 1.000000000000000000, 0.000000000000000000 ) ) ;
#3920 = ORIENTED_EDGE ( 'NONE', *, *, #6520, .F. ) ;
#3921 = CARTESIAN_POINT ( 'NONE',  ( -62.43234176562499016, 12.49479166632526805, 2.248837904296538071 ) ) ;
#3922 = CARTESIAN_POINT ( 'NONE',  ( -61.13531646874998415, 10.05729166632526983, 1.999225269531026417 ) ) ;
#3923 = CARTESIAN_POINT ( 'NONE',  ( -60.99999999999998579, 11.75000000000000000, 1.500000000000002220 ) ) ;
#3924 = EDGE_LOOP ( 'NONE', ( #9884, #7845, #4646, #7601 ) ) ;
#3925 = CARTESIAN_POINT ( 'NONE',  ( -62.49999999999998579, 12.16666666666666607, 2.366025403784441483 ) ) ;
#3926 = CARTESIAN_POINT ( 'NONE',  ( -61.99999999999998579, 11.03124999931720218, 0.5000000000000013323 ) ) ;
#3927 = EDGE_CURVE ( 'NONE', #6224, #5880, #255, .T. ) ;
#3928 = CARTESIAN_POINT ( 'NONE',  ( -61.49999999999998579, 12.26041666598386826, 0.6339745962155628467 ) ) ;
#3929 = EDGE_CURVE ( 'NONE', #10050, #4452, #4019, .T. ) ;
#3930 = DIRECTION ( 'NONE',  ( -1.000000000000000000, 0.000000000000000000, 0.000000000000000000 ) ) ;
#3931 = CARTESIAN_POINT ( 'NONE',  ( -61.13531646874998415, 13.05729166632526628, 1.999225269531026417 ) ) ;
#3932 = ADVANCED_FACE ( 'NONE', ( #10495 ), #8007, .F. ) ;
#3933 = ORIENTED_EDGE ( 'NONE', *, *, #10027, .T. ) ;
#3934 = CARTESIAN_POINT ( 'NONE',  ( -61.13531646874998415, 11.86979166632526805, 1.999225269531026417 ) ) ;
#3935 = CARTESIAN_POINT ( 'NONE',  ( -61.73205080756886076, 12.16741454900183506, 2.500000000000003109 ) ) ;
#3936 = DIRECTION ( 'NONE',  ( -1.000000000000000000, 0.000000000000000000, 0.000000000000000000 ) ) ;
#3937 = ORIENTED_EDGE ( 'NONE', *, *, #2980, .F. ) ;
#3938 = DIRECTION ( 'NONE',  ( 0.000000000000000000, -1.000000000000000000, 0.000000000000000000 ) ) ;
#3939 = CIRCLE ( 'NONE', #2884, 1.000000000000000888 ) ;
#3940 = ADVANCED_FACE ( 'NONE', ( #7116 ), #1223, .F. ) ;
#3941 = EDGE_LOOP ( 'NONE', ( #5298, #5003, #7576, #5126, #9431, #6674, #5871, #3855 ) ) ;
#3942 = CARTESIAN_POINT ( 'NONE',  ( -60.99999999999998579, 8.739583332650536107, 0.9226497308103762673 ) ) ;
#3943 = CARTESIAN_POINT ( 'NONE',  ( -61.49999999999998579, 10.20833333333333393, 2.366025403784441927 ) ) ;
#3944 = CARTESIAN_POINT ( 'NONE',  ( -62.26794919243111082, 9.542414549001833279, 0.4999999999999998890 ) ) ;
#3945 = CARTESIAN_POINT ( 'NONE',  ( -61.99999999999998579, 15.78124999931720218, 0.5000000000000013323 ) ) ;
#3946 = DIRECTION ( 'NONE',  ( -1.000000000000000000, -0.000000000000000000, -0.000000000000000000 ) ) ;
#3947 = CARTESIAN_POINT ( 'NONE',  ( -61.49999999999998579, 8.427083332650536107, 2.366025403784441927 ) ) ;
#3948 = MECHANICAL_DESIGN_GEOMETRIC_PRESENTATION_REPRESENTATION (  '', ( #2525 ), #6614 ) ;
#3949 = AXIS2_PLACEMENT_3D ( 'NONE', #10889, #1613, #2387 ) ;
#3950 = CARTESIAN_POINT ( 'NONE',  ( -61.56765823437498142, 11.93229166632526805, 0.7511620957034663704 ) ) ;
#3951 = CARTESIAN_POINT ( 'NONE',  ( -61.13531646874998415, 8.078124999658601979, 1.500000000000002220 ) ) ;
#3952 = VERTEX_POINT ( 'NONE', #5492 ) ;
#3953 = ADVANCED_FACE ( 'NONE', ( #1105, #4489 ), #7053, .F. ) ;
#3954 = LINE ( 'NONE', #8285, #4605 ) ;
#3955 = DIRECTION ( 'NONE',  ( -0.000000000000000000, 1.000000000000000000, 0.000000000000000000 ) ) ;
#3956 =( BOUNDED_CURVE ( )  B_SPLINE_CURVE ( 2, ( #5469, #3287, #4644, #1266, #8047, #436, #5840, #3820, #8105 ),
 .UNSPECIFIED., .F., .F. ) 
 B_SPLINE_CURVE_WITH_KNOTS ( ( 3, 2, 2, 2, 3 ),
 ( 0.7578125000000000000, 0.7604166666666666297, 0.7656250000000000000, 0.7708333333333333703, 0.7734375000000000000 ),
 .UNSPECIFIED. ) 
 CURVE ( )  GEOMETRIC_REPRESENTATION_ITEM ( )  RATIONAL_B_SPLINE_CURVE ( ( 0.9330127018922194093, 0.9330127018922194093, 1.000000000000000000, 0.8660254037844387076, 1.000000000000000000, 0.8660254037844387076, 1.000000000000000000, 0.9330127018922194093, 0.9330127018922194093 ) ) 
 REPRESENTATION_ITEM ( '' )  );
#3957 = ADVANCED_FACE ( 'NONE', ( #5257 ), #1163, .F. ) ;
#3958 = VERTEX_POINT ( 'NONE', #2950 ) ;
#3959 = CARTESIAN_POINT ( 'NONE',  ( -105.0000000000000000, -2.500000000000000000, 4.000000000000000000 ) ) ;
#3960 = CARTESIAN_POINT ( 'NONE',  ( -61.13531646874998415, 14.07812499965860198, 1.500000000000002220 ) ) ;
#3961 = PRESENTATION_LAYER_ASSIGNMENT (  '', '', ( #8755 ) ) ;
#3962 = CARTESIAN_POINT ( 'NONE',  ( -61.13531646874997705, 9.848958332991934128, 1.000774730468978468 ) ) ;
#3963 = CARTESIAN_POINT ( 'NONE',  ( -61.99999999999998579, 8.187500000000001776, 2.500000000000003109 ) ) ;
#3964 = VERTEX_POINT ( 'NONE', #1043 ) ;
#3965 = PLANE ( 'NONE',  #9538 ) ;
#3966 = CARTESIAN_POINT ( 'NONE',  ( -61.13531646874997705, 11.41145833299193590, 1.000774730468978468 ) ) ;
#3967 = CARTESIAN_POINT ( 'NONE',  ( -61.99999999999998579, 14.82812499965860020, 2.498450539062049724 ) ) ;
#3968 = ITEM_DEFINED_TRANSFORMATION ( 'NONE', 'NONE', #8696,  #2307 ) ;
#3969 = PLANE ( 'NONE',  #5656 ) ;
#3970 = EDGE_CURVE ( 'NONE', #10876, #4311, #1943, .T. ) ;
#3971 = CARTESIAN_POINT ( 'NONE',  ( -61.49999999999998579, 15.76041666598386826, 0.6339745962155628467 ) ) ;
#3972 = FACE_BOUND ( 'NONE', #5458, .T. ) ;
#3973 = VERTEX_POINT ( 'NONE', #9783 ) ;
#3974 = AXIS2_PLACEMENT_3D ( 'NONE', #6425, #2923, #10694 ) ;
#3975 = DIRECTION ( 'NONE',  ( 0.000000000000000000, 0.000000000000000000, -1.000000000000000000 ) ) ;
#3976 = DIRECTION ( 'NONE',  ( 0.000000000000000000, 0.000000000000000000, 1.000000000000000000 ) ) ;
#3977 = CARTESIAN_POINT ( 'NONE',  ( -62.43234176562498305, 14.41145833299193413, 0.7511620957034662593 ) ) ;
#3978 = CARTESIAN_POINT ( 'NONE',  ( -61.56765823437498142, 10.36979166632526983, 0.7511620957034663704 ) ) ;
#3979 = DIRECTION ( 'NONE',  ( 0.000000000000000000, 0.000000000000000000, -1.000000000000000000 ) ) ;
#3980 = ORIENTED_EDGE ( 'NONE', *, *, #10692, .F. ) ;
#3981 = CARTESIAN_POINT ( 'NONE',  ( -62.49999999999998579, 14.08333333333333393, 0.6339745962155627357 ) ) ;
#3982 = CIRCLE ( 'NONE', #10167, 25.99999999999999645 ) ;
#3983 = DIRECTION ( 'NONE',  ( 1.000000000000000000, 0.000000000000000000, 0.000000000000000000 ) ) ;
#3984 = CARTESIAN_POINT ( 'NONE',  ( -60.99999999999998579, 11.98958333265053433, 0.9226497308103762673 ) ) ;
#3985 = CARTESIAN_POINT ( 'NONE',  ( 0.3600944671415647336, -0.2500000000000001665, 1.887947737020719163 ) ) ;
#3986 = CARTESIAN_POINT ( 'NONE',  ( -62.86468353124999453, 13.45312499965860020, 1.500000000000002220 ) ) ;
#3987 = ORIENTED_EDGE ( 'NONE', *, *, #283, .T. ) ;
#3988 = EDGE_CURVE ( 'NONE', #562, #7309, #8556, .T. ) ;
#3989 = CARTESIAN_POINT ( 'NONE',  ( -62.43234176562498305, 11.72395833299193590, 0.7511620957034662593 ) ) ;
#3990 = CARTESIAN_POINT ( 'NONE',  ( -61.99999999999998579, 16.00000000000000000, 0.5000000000000041078 ) ) ;
#3991 = CARTESIAN_POINT ( 'NONE',  ( -61.99999999999998579, 15.82812499965860020, 2.498450539062049724 ) ) ;
#3992 = ORIENTED_EDGE ( 'NONE', *, *, #107, .T. ) ;
#3993 = CARTESIAN_POINT ( 'NONE',  ( -61.99999999999998579, 11.06250000000000000, 0.5000000000000013323 ) ) ;
#3994 = VERTEX_POINT ( 'NONE', #451 ) ;
#3995 = CARTESIAN_POINT ( 'NONE',  ( -62.99999999999998579, 9.864583332650536107, 2.077350269189627952 ) ) ;
#3996 = CARTESIAN_POINT ( 'NONE',  ( -60.99999999999998579, 9.770833333333332149, 0.9226497308103762673 ) ) ;
#3997 = LINE ( 'NONE', #10969, #3602 ) ;
#3998 = FACE_OUTER_BOUND ( 'NONE', #3941, .T. ) ;
#3999 = CARTESIAN_POINT ( 'NONE',  ( -61.99999999999998579, 15.81250000000000000, 0.5000000000000013323 ) ) ;
#4000 = CARTESIAN_POINT ( 'NONE',  ( -60.99999999999998579, 8.468749999317202182, 1.500000000000002220 ) ) ;
#4001 = EDGE_CURVE ( 'NONE', #5880, #4509, #3835, .T. ) ;
#4002 = CARTESIAN_POINT ( 'NONE',  ( -61.13531646874998415, 12.16145833299193413, 1.000774730468978468 ) ) ;
#4003 = DIRECTION ( 'NONE',  ( 3.965082230804130220E-16, -1.000000000000000000, -0.000000000000000000 ) ) ;
#4004 = VERTEX_POINT ( 'NONE', #5314 ) ;
#4005 = CARTESIAN_POINT ( 'NONE',  ( -61.99999999999998579, 12.78124999931720218, 0.5000000000000013323 ) ) ;
#4006 = ORIENTED_EDGE ( 'NONE', *, *, #412, .F. ) ;
#4007 = DIRECTION ( 'NONE',  ( 0.000000000000000000, 0.000000000000000000, 1.000000000000000000 ) ) ;
#4008 = CARTESIAN_POINT ( 'NONE',  ( -61.56765823437498852, 14.03645833299193413, 2.248837904296538515 ) ) ;
#4009 = DIRECTION ( 'NONE',  ( -0.000000000000000000, -1.000000000000000000, -0.000000000000000000 ) ) ;
#4010 = LINE ( 'NONE', #9019, #4752 ) ;
#4011 = CARTESIAN_POINT ( 'NONE',  ( -61.56765823437498142, 10.93229166632526805, 0.7511620957034663704 ) ) ;
#4012 = CARTESIAN_POINT ( 'NONE',  ( -61.99999999999998579, 15.32812499965860198, 2.498450539062049724 ) ) ;
#4013 = CARTESIAN_POINT ( 'NONE',  ( -62.99999999999998579, 13.61458333265053611, 2.077350269189627952 ) ) ;
#4014 = CARTESIAN_POINT ( 'NONE',  ( -62.99999999999998579, 15.61458333265053611, 2.077350269189627952 ) ) ;
#4015 = DIRECTION ( 'NONE',  ( 0.000000000000000000, 0.000000000000000000, 1.000000000000000000 ) ) ;
#4016 = ORIENTED_EDGE ( 'NONE', *, *, #5528, .F. ) ;
#4017 = CARTESIAN_POINT ( 'NONE',  ( -78.99999999999998579, 11.49999999999999645, 5.000000000000000000 ) ) ;
#4018 = DIRECTION ( 'NONE',  ( -0.000000000000000000, -0.000000000000000000, -1.000000000000000000 ) ) ;
#4019 =( BOUNDED_CURVE ( )  B_SPLINE_CURVE ( 2, ( #217, #8836, #3657, #4542, #7948, #2001, #1283, #4660, #8725 ),
 .UNSPECIFIED., .F., .T. ) 
 B_SPLINE_CURVE_WITH_KNOTS ( ( 3, 2, 2, 2, 3 ),
 ( 0.8515625000000000000, 0.8541666666666666297, 0.8593750000000000000, 0.8645833333333333703, 0.8671875000000000000 ),
 .UNSPECIFIED. ) 
 CURVE ( )  GEOMETRIC_REPRESENTATION_ITEM ( )  RATIONAL_B_SPLINE_CURVE ( ( 0.9330127018922194093, 0.9330127018922194093, 1.000000000000000000, 0.8660254037844387076, 1.000000000000000000, 0.8660254037844387076, 1.000000000000000000, 0.9330127018922194093, 0.9330127018922194093 ) ) 
 REPRESENTATION_ITEM ( '' )  );
#4020 = CARTESIAN_POINT ( 'NONE',  ( -61.56765823437498142, 13.86979166632526805, 0.7511620957034663704 ) ) ;
#4021 = EDGE_CURVE ( 'NONE', #8978, #8323, #8219, .T. ) ;
#4022 = CARTESIAN_POINT ( 'NONE',  ( -62.86468353124999453, 10.45312499965860198, 1.500000000000002220 ) ) ;
#4023 = CARTESIAN_POINT ( 'NONE',  ( 195.0000000000000000, -2.500000000000000000, 4.000000000000000000 ) ) ;
#4024 = ORIENTED_EDGE ( 'NONE', *, *, #9521, .T. ) ;
#4025 = CARTESIAN_POINT ( 'NONE',  ( -61.99999999999998579, 13.93750000000000000, 2.654700538379254571 ) ) ;
#4026 = CARTESIAN_POINT ( 'NONE',  ( -120.0000000000000000, 8.000000000000000000, 3.000000000000000000 ) ) ;
#4027 = CARTESIAN_POINT ( 'NONE',  ( -61.49999999999998579, 11.67708333265053611, 2.366025403784441927 ) ) ;
#4028 = CARTESIAN_POINT ( 'NONE',  ( -61.56765823437498142, 13.86979166632526805, 0.7511620957034663704 ) ) ;
#4029 = ADVANCED_FACE ( 'NONE', ( #6563 ), #6506, .T. ) ;
#4030 = VERTEX_POINT ( 'NONE', #9160 ) ;
#4031 = CARTESIAN_POINT ( 'NONE',  ( -61.99999999999998579, 11.57812499965860198, 2.498450539062049724 ) ) ;
#4032 = DIRECTION ( 'NONE',  ( -1.000000000000000000, 0.000000000000000000, 0.000000000000000000 ) ) ;
#4033 = CIRCLE ( 'NONE', #4565, 5.000000000000004441 ) ;
#4034 = PRODUCT_DEFINITION_SHAPE ( 'NONE', 'NONE',  #5343 ) ;
#4035 = CARTESIAN_POINT ( 'NONE',  ( 145.0000000000000284, 5.500000000000000000, 3.000000000000000000 ) ) ;
#4036 = ORIENTED_EDGE ( 'NONE', *, *, #2056, .F. ) ;
#4037 = CARTESIAN_POINT ( 'NONE',  ( 0.000000000000000000, 0.000000000000000000, 0.000000000000000000 ) ) ;
#4038 = EDGE_CURVE ( 'NONE', #10017, #4689, #2893, .T. ) ;
#4039 = AXIS2_PLACEMENT_3D ( 'NONE', #6137, #1862, #6757 ) ;
#4040 = ORIENTED_EDGE ( 'NONE', *, *, #7580, .T. ) ;
#4041 = CARTESIAN_POINT ( 'NONE',  ( -62.49999999999998579, 9.802083332650536107, 0.6339745962155627357 ) ) ;
#4042 = CARTESIAN_POINT ( 'NONE',  ( -62.99999999999998579, 9.375000000000000000, 1.500000000000001998 ) ) ;
#4043 = VECTOR ( 'NONE', #820, 1000.000000000000000 ) ;
#4044 = CARTESIAN_POINT ( 'NONE',  ( -62.43234176562498305, 8.223958332991934128, 0.7511620957034662593 ) ) ;
#4045 = CARTESIAN_POINT ( 'NONE',  ( -60.99999999999998579, 15.48958333265053433, 0.9226497308103762673 ) ) ;
#4046 = EDGE_CURVE ( 'NONE', #4413, #1330, #8953, .T. ) ;
#4047 = MECHANICAL_DESIGN_GEOMETRIC_PRESENTATION_REPRESENTATION (  '', ( #5815 ), #2816 ) ;
#4048 = CARTESIAN_POINT ( 'NONE',  ( -61.56765823437498852, 11.34895833299193590, 2.248837904296538515 ) ) ;
#4049 = CARTESIAN_POINT ( 'NONE',  ( -61.99999999999998579, 14.65624999931719863, 2.500000000000002665 ) ) ;
#4050 = ORIENTED_EDGE ( 'NONE', *, *, #7024, .T. ) ;
#4051 = CARTESIAN_POINT ( 'NONE',  ( -62.99999999999998579, 15.35416666666666785, 0.9226497308103756012 ) ) ;
#4052 = EDGE_CURVE ( 'NONE', #5466, #5034, #674, .T. ) ;
#4053 = AXIS2_PLACEMENT_3D ( 'NONE', #6840, #2611, #10109 ) ;
#4054 = VERTEX_POINT ( 'NONE', #8120 ) ;
#4055 = DIRECTION ( 'NONE',  ( 0.000000000000000000, 0.000000000000000000, 1.000000000000000000 ) ) ;
#4056 = ADVANCED_FACE ( 'NONE', ( #5710 ), #1497, .T. ) ;
#4057 = CARTESIAN_POINT ( 'NONE',  ( -61.56765823437498142, 13.36979166632526805, 0.7511620957034663704 ) ) ;
#4058 = AXIS2_PLACEMENT_3D ( 'NONE', #9334, #7732, #8404 ) ;
#4059 = LINE ( 'NONE', #7459, #6627 ) ;
#4060 = CARTESIAN_POINT ( 'NONE',  ( -62.49999999999998579, 14.16666666666666785, 2.366025403784441483 ) ) ;
#4061 = CARTESIAN_POINT ( 'NONE',  ( -61.13531646874997705, 12.36979166632526805, 1.999225269531026417 ) ) ;
#4062 = CARTESIAN_POINT ( 'NONE',  ( -62.86468353124998032, 15.74479166632526805, 1.000774730468978246 ) ) ;
#4064 = DIRECTION ( 'NONE',  ( 0.000000000000000000, 0.000000000000000000, -1.000000000000000000 ) ) ;
#4063 = PRODUCT_RELATED_PRODUCT_CATEGORY ( 'part', '', ( #7328 ) ) ;
#4065 = CARTESIAN_POINT ( 'NONE',  ( -62.99999999999998579, 15.10416666666666607, 0.9226497308103756012 ) ) ;
#4066 = CARTESIAN_POINT ( 'NONE',  ( -62.86468353124999453, 8.265624999658601979, 1.500000000000002220 ) ) ;
#4067 = DIRECTION ( 'NONE',  ( -1.000000000000000000, -0.000000000000000000, -0.000000000000000000 ) ) ;
#4068 = ORIENTED_EDGE ( 'NONE', *, *, #8863, .T. ) ;
#4069 = DIRECTION ( 'NONE',  ( -1.000000000000000000, 0.000000000000000000, 0.000000000000000000 ) ) ;
#4070 = DIRECTION ( 'NONE',  ( -0.000000000000000000, 1.000000000000000000, -0.000000000000000000 ) ) ;
#4071 = VECTOR ( 'NONE', #2045, 1000.000000000000000 ) ;
#4072 = STYLED_ITEM ( 'NONE', ( #8631 ), #2558 ) ;
#4073 = CARTESIAN_POINT ( 'NONE',  ( -61.99999999999999289, 13.76562499965860198, 2.498450539062049724 ) ) ;
#4074 = CARTESIAN_POINT ( 'NONE',  ( -61.99999999999998579, 9.890624999658601979, 0.5015494609379544944 ) ) ;
#4075 = CARTESIAN_POINT ( 'NONE',  ( -61.13531646874998415, 8.078124999658601979, 1.500000000000002220 ) ) ;
#4076 = FACE_OUTER_BOUND ( 'NONE', #3911, .T. ) ;
#4077 = ORIENTED_EDGE ( 'NONE', *, *, #3927, .F. ) ;
#4078 = CARTESIAN_POINT ( 'NONE',  ( -62.99999999999998579, 13.35416666666666785, 0.9226497308103756012 ) ) ;
#4079 = CARTESIAN_POINT ( 'NONE',  ( -62.86468353124999453, 9.265624999658600203, 1.500000000000002220 ) ) ;
#4080 = VECTOR ( 'NONE', #4780, 1000.000000000000000 ) ;
#4081 = FILL_AREA_STYLE ('',( #698 ) ) ;
#4082 = CARTESIAN_POINT ( 'NONE',  ( -61.49999999999998579, 12.51041666598386826, 0.6339745962155628467 ) ) ;
#4083 = ORIENTED_EDGE ( 'NONE', *, *, #7073, .F. ) ;
#4084 =( BOUNDED_CURVE ( )  B_SPLINE_CURVE ( 2, ( #6616, #4097, #9994, #6457, #1544, #4926, #8324, #3109, #9839 ),
 .UNSPECIFIED., .F., .T. ) 
 B_SPLINE_CURVE_WITH_KNOTS ( ( 3, 2, 2, 2, 3 ),
 ( 0.1484374999999999722, 0.1510416666666666574, 0.1562500000000000000, 0.1614583333333333426, 0.1640624999999999722 ),
 .UNSPECIFIED. ) 
 CURVE ( )  GEOMETRIC_REPRESENTATION_ITEM ( )  RATIONAL_B_SPLINE_CURVE ( ( 0.9330127018922194093, 0.9330127018922186322, 1.000000000000000000, 0.8660254037844387076, 1.000000000000000000, 0.8660254037844387076, 1.000000000000000000, 0.9330127018922200755, 0.9330127018922194093 ) ) 
 REPRESENTATION_ITEM ( '' )  );
#4085 = FILL_AREA_STYLE ('',( #2578 ) ) ;
#4086 = CARTESIAN_POINT ( 'NONE',  ( -61.13531646874998415, 13.57812499965860198, 1.500000000000002220 ) ) ;
#4087 = EDGE_CURVE ( 'NONE', #4203, #7478, #9887, .T. ) ;
#4088 = ORIENTED_EDGE ( 'NONE', *, *, #1610, .T. ) ;
#4089 = CARTESIAN_POINT ( 'NONE',  ( -62.86468353124998032, 11.24479166632526805, 1.000774730468978246 ) ) ;
#4090 = LINE ( 'NONE', #6761, #8317 ) ;
#4091 = EDGE_CURVE ( 'NONE', #6875, #4509, #7782, .T. ) ;
#4092 = ADVANCED_FACE ( 'NONE', ( #7390 ), #10725, .T. ) ;
#4093 = DIRECTION ( 'NONE',  ( 0.000000000000000000, 0.000000000000000000, -1.000000000000000000 ) ) ;
#4094 = ORIENTED_EDGE ( 'NONE', *, *, #362, .F. ) ;
#4095 = DIRECTION ( 'NONE',  ( -1.000000000000000000, 0.000000000000000000, 0.000000000000000000 ) ) ;
#4096 = ORIENTED_EDGE ( 'NONE', *, *, #960, .T. ) ;
#4097 = CARTESIAN_POINT ( 'NONE',  ( -61.73205080756886787, 9.417414549001833279, 2.500000000000004885 ) ) ;
#4098 = CARTESIAN_POINT ( 'NONE',  ( -60.99999999999998579, 11.50000000000000000, 1.500000000000002220 ) ) ;
#4099 = CARTESIAN_POINT ( 'NONE',  ( -61.99999999999998579, 9.781249999317202182, 0.5000000000000013323 ) ) ;
#4100 = DIRECTION ( 'NONE',  ( 0.000000000000000000, -0.000000000000000000, 1.000000000000000000 ) ) ;
#4101 = CARTESIAN_POINT ( 'NONE',  ( -61.99999999999998579, 9.406249999317202182, 2.654700538379254571 ) ) ;
#4102 = CARTESIAN_POINT ( 'NONE',  ( -62.86468353124999453, 12.76562499965860198, 1.500000000000002220 ) ) ;
#4103 = CARTESIAN_POINT ( 'NONE',  ( -62.49999999999998579, 10.58333333333333393, 0.6339745962155627357 ) ) ;
#4104 = ORIENTED_EDGE ( 'NONE', *, *, #1718, .T. ) ;
#4105 = CIRCLE ( 'NONE', #6779, 1.000000000000000000 ) ;
#4106 = CARTESIAN_POINT ( 'NONE',  ( -62.26794919243111082, 15.42633545031536713, 2.500000000000003109 ) ) ;
#4107 = ORIENTED_EDGE ( 'NONE', *, *, #901, .F. ) ;
#4108 = CARTESIAN_POINT ( 'NONE',  ( 140.0000000000000568, -2.500000000000000000, 4.000000000000000000 ) ) ;
#4109 = EDGE_CURVE ( 'NONE', #5909, #2359, #4084, .T. ) ;
#4110 = CARTESIAN_POINT ( 'NONE',  ( -62.86468353124998032, 14.68229166632526805, 1.000774730468978246 ) ) ;
#4111 = CARTESIAN_POINT ( 'NONE',  ( -60.99999999999998579, 13.72916666666666785, 2.077350269189628840 ) ) ;
#4112 = CARTESIAN_POINT ( 'NONE',  ( -60.99999999999998579, 14.49999999999999822, 1.500000000000002220 ) ) ;
#4113 = FACE_OUTER_BOUND ( 'NONE', #7569, .T. ) ;
#4114 = CIRCLE ( 'NONE', #37, 20.00000000000000355 ) ;
#4115 = CARTESIAN_POINT ( 'NONE',  ( -61.13531646874997705, 13.36979166632526805, 1.999225269531026417 ) ) ;
#4116 = CARTESIAN_POINT ( 'NONE',  ( -62.43234176562499016, 15.30729166632526805, 2.248837904296538071 ) ) ;
#4117 = ADVANCED_FACE ( 'NONE', ( #716 ), #10877, .F. ) ;
#4118 = CARTESIAN_POINT ( 'NONE',  ( -114.9999999999999147, -43.00000000000000000, -2.000000000000000000 ) ) ;
#4119 = CONTEXT_DEPENDENT_SHAPE_REPRESENTATION ( #542, #2627 ) ;
#4120 = CARTESIAN_POINT ( 'NONE',  ( -119.9999999999999716, 8.000000000000001776, 0.000000000000000000 ) ) ;
#4121 = CARTESIAN_POINT ( 'NONE',  ( -61.99999999999998579, 16.15624999931720396, 2.654700538379254571 ) ) ;
#4122 = DIRECTION ( 'NONE',  ( 0.000000000000000000, 1.000000000000000000, 0.000000000000000000 ) ) ;
#4123 = ORIENTED_EDGE ( 'NONE', *, *, #6104, .T. ) ;
#4124 = CARTESIAN_POINT ( 'NONE',  ( -144.9999999999999147, -16.54248688935410883, -2.000000000000000000 ) ) ;
#4125 = CARTESIAN_POINT ( 'NONE',  ( -105.0000000000000000, 2.500000000000000000, 4.000000000000000000 ) ) ;
#4126 = VECTOR ( 'NONE', #3138, 1000.000000000000000 ) ;
#4127 = VECTOR ( 'NONE', #10514, 1000.000000000000000 ) ;
#4128 = CARTESIAN_POINT ( 'NONE',  ( -61.56765823437498852, 14.53645833299193413, 2.248837904296538515 ) ) ;
#4129 = CARTESIAN_POINT ( 'NONE',  ( -61.13531646874998415, 9.828124999658601979, 1.500000000000002220 ) ) ;
#4130 = CARTESIAN_POINT ( 'NONE',  ( -61.99999999999999289, 15.20312499965860020, 0.5015494609379544944 ) ) ;
#4131 = CARTESIAN_POINT ( 'NONE',  ( -61.99999999999998579, 26.00000000000000355, 1.500000000000002220 ) ) ;
#4132 = EDGE_LOOP ( 'NONE', ( #5405, #2319, #1557, #4656 ) ) ;
#4133 = CARTESIAN_POINT ( 'NONE',  ( -60.99999999999998579, 13.75000000000000000, 1.500000000000002220 ) ) ;
#4134 = CARTESIAN_POINT ( 'NONE',  ( -62.43234176562498305, 8.723958332991934128, 0.7511620957034662593 ) ) ;
#4135 = SURFACE_STYLE_USAGE ( .BOTH. , #5801 ) ;
#4136 = CARTESIAN_POINT ( 'NONE',  ( -60.99999999999998579, 12.23958333265053611, 0.9226497308103762673 ) ) ;
#4137 = ADVANCED_FACE ( 'NONE', ( #2226 ), #5605, .T. ) ;
#4138 = VECTOR ( 'NONE', #7055, 1000.000000000000000 ) ;
#4139 = CARTESIAN_POINT ( 'NONE',  ( -61.13531646874998415, 14.05729166632526805, 1.999225269531026417 ) ) ;
#4140 = CARTESIAN_POINT ( 'NONE',  ( 190.0000000000000000, 2.500000000000000000, 4.000000000000000000 ) ) ;
#4141 = ORIENTED_EDGE ( 'NONE', *, *, #6023, .T. ) ;
#4142 = CARTESIAN_POINT ( 'NONE',  ( -61.13531646874998415, 12.86979166632526628, 1.999225269531026417 ) ) ;
#4143 =( BOUNDED_CURVE ( )  B_SPLINE_CURVE ( 2, ( #6833, #8496, #10935, #3326, #828, #3487, #9491, #1775, #6727 ),
 .UNSPECIFIED., .F., .T. ) 
 B_SPLINE_CURVE_WITH_KNOTS ( ( 3, 2, 2, 2, 3 ),
 ( 0.5859375000000000000, 0.5885416666666666297, 0.5937500000000000000, 0.5989583333333333703, 0.6015625000000000000 ),
 .UNSPECIFIED. ) 
 CURVE ( )  GEOMETRIC_REPRESENTATION_ITEM ( )  RATIONAL_B_SPLINE_CURVE ( ( 0.9330127018922194093, 0.9330127018922194093, 1.000000000000000000, 0.8660254037844387076, 1.000000000000000000, 0.8660254037844387076, 1.000000000000000000, 0.9330127018922194093, 0.9330127018922194093 ) ) 
 REPRESENTATION_ITEM ( '' )  );
#4144 = DIRECTION ( 'NONE',  ( -0.000000000000000000, -1.000000000000000000, -0.000000000000000000 ) ) ;
#4145 = ORIENTED_EDGE ( 'NONE', *, *, #7194, .F. ) ;
#4146 = DIRECTION ( 'NONE',  ( -0.000000000000000000, -1.000000000000000000, -0.000000000000000000 ) ) ;
#4147 = ORIENTED_EDGE ( 'NONE', *, *, #8394, .F. ) ;
#4148 = CARTESIAN_POINT ( 'NONE',  ( -61.99999999999998579, 11.56250000000000000, 0.3452994616207497591 ) ) ;
#4149 = ORIENTED_EDGE ( 'NONE', *, *, #1877, .T. ) ;
#4150 = CARTESIAN_POINT ( 'NONE',  ( -62.86468353124998032, 9.494791666325269830, 1.000774730468978246 ) ) ;
#4151 = CARTESIAN_POINT ( 'NONE',  ( -61.99999999999998579, 16.00000000000000000, 2.500000000000000444 ) ) ;
#4152 = CARTESIAN_POINT ( 'NONE',  ( -61.99999999999998579, 12.70312499965860198, 0.5015494609379544944 ) ) ;
#4153 = CARTESIAN_POINT ( 'NONE',  ( -62.49999999999998579, 9.135416665983868256, 2.366025403784441483 ) ) ;
#4154 = ORIENTED_EDGE ( 'NONE', *, *, #9639, .T. ) ;
#4155 = CARTESIAN_POINT ( 'NONE',  ( -120.0000000000000000, 14.99999999999998579, 5.000000000000004441 ) ) ;
#4156 = ORIENTED_EDGE ( 'NONE', *, *, #2436, .T. ) ;
#4157 = CARTESIAN_POINT ( 'NONE',  ( -120.0000000000000000, -4.000000000000019540, 0.000000000000000000 ) ) ;
#4158 = CARTESIAN_POINT ( 'NONE',  ( -62.86468353124999453, 14.70312499965860020, 1.500000000000002220 ) ) ;
#4159 = CARTESIAN_POINT ( 'NONE',  ( -61.99999999999998579, 9.531249999317202182, 0.5000000000000013323 ) ) ;
#4160 = CARTESIAN_POINT ( 'NONE',  ( -120.0000000000000000, -4.000000000000019540, -2.000000000000000000 ) ) ;
#4161 = CARTESIAN_POINT ( 'NONE',  ( -62.99999999999998579, 12.32291666598386826, 0.9226497308103756012 ) ) ;
#4162 = CARTESIAN_POINT ( 'NONE',  ( -61.56765823437498852, 12.59895833299193413, 2.248837904296538515 ) ) ;
#4163 = CARTESIAN_POINT ( 'NONE',  ( -61.13531646874998415, 15.66145833299193590, 1.000774730468978468 ) ) ;
#4164 = CARTESIAN_POINT ( 'NONE',  ( -61.49999999999998579, 15.04166666666666607, 0.6339745962155628467 ) ) ;
#4165 = DIRECTION ( 'NONE',  ( 0.000000000000000000, 0.000000000000000000, 1.000000000000000000 ) ) ;
#4166 = CARTESIAN_POINT ( 'NONE',  ( -62.86468353124999453, 9.015624999658601979, 1.500000000000002220 ) ) ;
#4167 = CARTESIAN_POINT ( 'NONE',  ( -61.99999999999998579, -8.000000000000000000, 1.500000000000002220 ) ) ;
#4168 = ORIENTED_EDGE ( 'NONE', *, *, #4109, .T. ) ;
#4169 = DIRECTION ( 'NONE',  ( -0.7071067811865472397, 8.659560562354929160E-17, 0.7071067811865479058 ) ) ;
#4170 = FACE_OUTER_BOUND ( 'NONE', #7161, .T. ) ;
#4171 = EDGE_CURVE ( 'NONE', #3478, #8518, #3590, .T. ) ;
#4172 = CARTESIAN_POINT ( 'NONE',  ( -61.13531646874997705, 14.59895833299193413, 1.000774730468978468 ) ) ;
#4173 = CARTESIAN_POINT ( 'NONE',  ( -62.86468353124998742, 10.97395833299193768, 1.999225269531025972 ) ) ;
#4174 = CARTESIAN_POINT ( 'NONE',  ( -61.13531646874997705, 15.11979166632526983, 1.999225269531026417 ) ) ;
#4175 = CARTESIAN_POINT ( 'NONE',  ( -60.99999999999998579, 14.46874999931720218, 1.500000000000002220 ) ) ;
#4176 = ORIENTED_EDGE ( 'NONE', *, *, #722, .F. ) ;
#4177 = CARTESIAN_POINT ( 'NONE',  ( -61.49999999999998579, 14.04166666666666785, 0.6339745962155628467 ) ) ;
#4178 = CARTESIAN_POINT ( 'NONE',  ( -61.99999999999999289, 8.578124999658601979, 2.498450539062049724 ) ) ;
#4179 = CARTESIAN_POINT ( 'NONE',  ( -60.99999999999998579, 12.98958333265053433, 0.9226497308103762673 ) ) ;
#4180 = EDGE_LOOP ( 'NONE', ( #1442, #7293, #5341, #7707 ) ) ;
#4181 = SURFACE_SIDE_STYLE ('',( #1643 ) ) ;
#4182 = CARTESIAN_POINT ( 'NONE',  ( -61.13531646874998415, 13.80729166632526983, 1.999225269531026417 ) ) ;
#4183 = CARTESIAN_POINT ( 'NONE',  ( -62.99999999999998579, 15.62500000000000000, 1.500000000000001998 ) ) ;
#4184 = VERTEX_POINT ( 'NONE', #3689 ) ;
#4185 = EDGE_CURVE ( 'NONE', #1245, #8943, #959, .T. ) ;
#4186 = DIRECTION ( 'NONE',  ( 1.000000000000000000, 0.000000000000000000, -0.000000000000000000 ) ) ;
#4187 = CARTESIAN_POINT ( 'NONE',  ( -62.43234176562499016, 12.30729166632526805, 2.248837904296538071 ) ) ;
#4188 = CARTESIAN_POINT ( 'NONE',  ( 150.0000000000000284, 2.500000000000000000, 3.000000000000000000 ) ) ;
#4189 = ORIENTED_EDGE ( 'NONE', *, *, #4091, .F. ) ;
#4190 = FACE_OUTER_BOUND ( 'NONE', #2741, .T. ) ;
#4191 = APPLICATION_CONTEXT ( 'automotive_design' ) ;
#4192 = VERTEX_POINT ( 'NONE', #2810 ) ;
#4193 = LINE ( 'NONE', #1657, #7636 ) ;
#4194 =( BOUNDED_CURVE ( )  B_SPLINE_CURVE ( 2, ( #6006, #66, #7907, #1958, #9565, #8622, #4381, #9394, #7794 ),
 .UNSPECIFIED., .F., .T. ) 
 B_SPLINE_CURVE_WITH_KNOTS ( ( 3, 2, 2, 2, 3 ),
 ( 0.3671875000000000000, 0.3697916666666666852, 0.3750000000000000000, 0.3802083333333333148, 0.3828124999999999445 ),
 .UNSPECIFIED. ) 
 CURVE ( )  GEOMETRIC_REPRESENTATION_ITEM ( )  RATIONAL_B_SPLINE_CURVE ( ( 0.9330127018922194093, 0.9330127018922194093, 1.000000000000000000, 0.8660254037844387076, 1.000000000000000000, 0.8660254037844387076, 1.000000000000000000, 0.9330127018922207416, 0.9330127018922192983 ) ) 
 REPRESENTATION_ITEM ( '' )  );
#4195 = ORIENTED_EDGE ( 'NONE', *, *, #3546, .T. ) ;
#4196 = CARTESIAN_POINT ( 'NONE',  ( -62.49999999999998579, 11.66666666666666785, 2.366025403784441483 ) ) ;
#4197 = AXIS2_PLACEMENT_3D ( 'NONE', #8886, #7996, #6444 ) ;
#4198 = VERTEX_POINT ( 'NONE', #7812 ) ;
#4199 = CARTESIAN_POINT ( 'NONE',  ( -62.43234176562499016, 8.307291666325268054, 2.248837904296538071 ) ) ;
#4200 = CARTESIAN_POINT ( 'NONE',  ( -61.73205080756886076, 10.52008544963257464, 0.5000000000000044409 ) ) ;
#4201 = CARTESIAN_POINT ( 'NONE',  ( -62.43234176562499016, 13.05729166632526805, 2.248837904296538071 ) ) ;
#4202 = CARTESIAN_POINT ( 'NONE',  ( -62.99999999999998579, 9.322916665983871809, 0.9226497308103756012 ) ) ;
#4203 = VERTEX_POINT ( 'NONE', #908 ) ;
#4204 = CARTESIAN_POINT ( 'NONE',  ( -60.99999999999998579, 10.96874999931720218, 1.500000000000002220 ) ) ;
#4205 = AXIS2_PLACEMENT_3D ( 'NONE', #1780, #3328, #2502 ) ;
#4206 = PRODUCT_DEFINITION_SHAPE ( 'NONE', 'NONE',  #10302 ) ;
#4207 = ORIENTED_EDGE ( 'NONE', *, *, #8822, .T. ) ;
#4208 = CARTESIAN_POINT ( 'NONE',  ( -62.43234176562499016, 14.74479166632526805, 2.248837904296538071 ) ) ;
#4209 = CARTESIAN_POINT ( 'NONE',  ( -37.99999999999999289, -14.00000000000000888, 5.000000000000000000 ) ) ;
#4210 = CARTESIAN_POINT ( 'NONE',  ( -61.73205080756886076, 12.44866454968463110, 2.500000000000003109 ) ) ;
#4211 = EDGE_CURVE ( 'NONE', #8978, #3194, #4522, .T. ) ;
#4212 = DIRECTION ( 'NONE',  ( 0.000000000000000000, 0.000000000000000000, 1.000000000000000000 ) ) ;
#4213 = CARTESIAN_POINT ( 'NONE',  ( -61.13531646874997705, 13.11979166632526805, 1.999225269531026417 ) ) ;
#4214 = CARTESIAN_POINT ( 'NONE',  ( -61.13531646874998415, 15.64062499965860198, 1.500000000000002220 ) ) ;
#4215 = CARTESIAN_POINT ( 'NONE',  ( -105.0000000000000000, 2.500000000000000000, 4.000000000000000000 ) ) ;
#4216 = CYLINDRICAL_SURFACE ( 'NONE', #6906, 1.000000000000000888 ) ;
#4217 = CARTESIAN_POINT ( 'NONE',  ( -62.43234176562498305, 9.723958332991934128, 0.7511620957034662593 ) ) ;
#4218 = DIRECTION ( 'NONE',  ( -0.000000000000000000, -1.000000000000000000, -0.000000000000000000 ) ) ;
#4219 = ORIENTED_EDGE ( 'NONE', *, *, #3016, .F. ) ;
#4220 = CARTESIAN_POINT ( 'NONE',  ( -61.99999999999998579, 16.00000000000000000, 0.5000000000000041078 ) ) ;
#4221 = EDGE_CURVE ( 'NONE', #3055, #10734, #2243, .T. ) ;
#4222 = DIRECTION ( 'NONE',  ( -1.000000000000000000, 0.000000000000000000, 0.000000000000000000 ) ) ;
#4223 = AXIS2_PLACEMENT_3D ( 'NONE', #8062, #558, #3936 ) ;
#4224 = CARTESIAN_POINT ( 'NONE',  ( -62.86468353124998032, 15.43229166632526805, 1.000774730468978024 ) ) ;
#4225 = CARTESIAN_POINT ( 'NONE',  ( -61.13531646874998415, 11.82812499965860198, 1.500000000000002220 ) ) ;
#4226 = CARTESIAN_POINT ( 'NONE',  ( -62.86468353124998032, 14.99479166632526628, 1.000774730468978024 ) ) ;
#4227 = CARTESIAN_POINT ( 'NONE',  ( -62.49999999999998579, 13.05208333265053611, 0.6339745962155627357 ) ) ;
#4228 = ORIENTED_EDGE ( 'NONE', *, *, #5091, .F. ) ;
#4229 = CARTESIAN_POINT ( 'NONE',  ( -62.49999999999998579, 15.33333333333333393, 0.6339745962155627357 ) ) ;
#4230 = CARTESIAN_POINT ( 'NONE',  ( -61.56765823437498142, 8.182291666325268054, 0.7511620957034663704 ) ) ;
#4231 = VECTOR ( 'NONE', #1523, 1000.000000000000000 ) ;
#4232 = CARTESIAN_POINT ( 'NONE',  ( -62.49999999999998579, 13.88541666598387003, 2.366025403784441483 ) ) ;
#4233 = ORIENTED_EDGE ( 'NONE', *, *, #9765, .F. ) ;
#4234 = STYLED_ITEM ( 'NONE', ( #2764 ), #4690 ) ;
#4235 = CARTESIAN_POINT ( 'NONE',  ( -61.99999999999999289, 11.01562499965859843, 2.498450539062049724 ) ) ;
#4236 = CARTESIAN_POINT ( 'NONE',  ( -120.0000000000000000, 14.99999999999998579, 5.000000000000004441 ) ) ;
#4237 = AXIS2_PLACEMENT_3D ( 'NONE', #3733, #2015, #231 ) ;
#4238 = VERTEX_POINT ( 'NONE', #8587 ) ;
#4239 = EDGE_CURVE ( 'NONE', #5427, #5356, #9469, .T. ) ;
#4240 = CARTESIAN_POINT ( 'NONE',  ( -62.49999999999998579, 12.91666666666666607, 2.366025403784441483 ) ) ;
#4241 = AXIS2_PLACEMENT_3D ( 'NONE', #10576, #1130, #3858 ) ;
#4242 = CARTESIAN_POINT ( 'NONE',  ( -62.43234176562498305, 13.47395833299193413, 0.7511620957034662593 ) ) ;
#4243 = DIRECTION ( 'NONE',  ( -1.000000000000000000, 0.000000000000000000, -0.000000000000000000 ) ) ;
#4244 = EDGE_CURVE ( 'NONE', #8518, #2471, #759, .T. ) ;
#4245 = EDGE_LOOP ( 'NONE', ( #7348, #2049, #442, #6615 ) ) ;
#4246 = DIRECTION ( 'NONE',  ( -0.000000000000000000, -0.000000000000000000, 1.000000000000000000 ) ) ;
#4247 = EDGE_LOOP ( 'NONE', ( #9993, #8057, #5079, #5148 ) ) ;
#4248 = DIRECTION ( 'NONE',  ( 0.000000000000000000, 0.000000000000000000, -1.000000000000000000 ) ) ;
#4249 = FILL_AREA_STYLE_COLOUR ( '', #1041 ) ;
#4250 = ORIENTED_EDGE ( 'NONE', *, *, #7867, .F. ) ;
#4251 = VERTEX_POINT ( 'NONE', #7031 ) ;
#4252 = CARTESIAN_POINT ( 'NONE',  ( -61.56765823437498852, 8.348958332991934128, 2.248837904296538515 ) ) ;
#4253 = CARTESIAN_POINT ( 'NONE',  ( -60.99999999999998579, 14.24999999999999822, 1.500000000000002220 ) ) ;
#4254 = CARTESIAN_POINT ( 'NONE',  ( -62.86468353124999453, 12.51562499965860198, 1.500000000000002220 ) ) ;
#4255 = CARTESIAN_POINT ( 'NONE',  ( -61.99999999999998579, 12.90624999931720218, 2.500000000000002665 ) ) ;
#4256 = ORIENTED_EDGE ( 'NONE', *, *, #9844, .F. ) ;
#4257 = CARTESIAN_POINT ( 'NONE',  ( -60.99999999999998579, 10.94791666598387181, 2.077350269189628840 ) ) ;
#4258 = EDGE_CURVE ( 'NONE', #5709, #8064, #6196, .T. ) ;
#4259 = ORIENTED_EDGE ( 'NONE', *, *, #10324, .F. ) ;
#4260 = CARTESIAN_POINT ( 'NONE',  ( 0.5000000000000000000, -0.2500000000000000000, 1.911797424705720116 ) ) ;
#4261 = CARTESIAN_POINT ( 'NONE',  ( -62.43234176562499016, 15.49479166632526628, 2.248837904296538071 ) ) ;
#4262 = CARTESIAN_POINT ( 'NONE',  ( -61.99999999999998579, 8.000000000000000000, 2.500000000000003109 ) ) ;
#4263 = CARTESIAN_POINT ( 'NONE',  ( -60.99999999999998579, 12.48958333265053611, 0.9226497308103762673 ) ) ;
#4264 = CARTESIAN_POINT ( 'NONE',  ( -62.26794919243111792, 8.823664549684632874, 0.5000000000000059952 ) ) ;
#4265 = CARTESIAN_POINT ( 'NONE',  ( -61.99999999999999289, 12.57812499965860198, 2.498450539062049724 ) ) ;
#4266 = CARTESIAN_POINT ( 'NONE',  ( -61.13531646874998415, 8.598958332991934128, 1.000774730468978468 ) ) ;
#4267 = LINE ( 'NONE', #4215, #3344 ) ;
#4268 = LINE ( 'NONE', #2612, #7441 ) ;
#4269 =( GEOMETRIC_REPRESENTATION_CONTEXT ( 3 ) GLOBAL_UNCERTAINTY_ASSIGNED_CONTEXT ( ( #9164 ) ) GLOBAL_UNIT_ASSIGNED_CONTEXT ( ( #897, #7743, #3507 ) ) REPRESENTATION_CONTEXT ( 'NONE', 'WORKASPACE' ) );
#4270 = CARTESIAN_POINT ( 'NONE',  ( -61.13531646874998415, 9.390624999658600203, 1.500000000000002220 ) ) ;
#4271 = EDGE_LOOP ( 'NONE', ( #4562, #1864, #7127, #6830 ) ) ;
#4272 = CARTESIAN_POINT ( 'NONE',  ( 150.0000000000000000, 8.000000000000000000, 6.000000000000000000 ) ) ;
#4273 = CARTESIAN_POINT ( 'NONE',  ( -61.73205080756886076, 12.91741454900183328, 2.500000000000003109 ) ) ;
#4274 = EDGE_CURVE ( 'NONE', #5256, #9156, #10409, .T. ) ;
#4275 = CARTESIAN_POINT ( 'NONE',  ( -61.13531646874998415, 15.57812499965860198, 1.500000000000002220 ) ) ;
#4276 = CARTESIAN_POINT ( 'NONE',  ( -62.86468353124999453, 10.95312499965860020, 1.500000000000002220 ) ) ;
#4277 = CARTESIAN_POINT ( 'NONE',  ( -61.13531646874997705, 15.36979166632526805, 1.999225269531026417 ) ) ;
#4278 = CARTESIAN_POINT ( 'NONE',  ( -77.99999999999998579, 0.000000000000000000, 13.00000000000000178 ) ) ;
#4279 = ORIENTED_EDGE ( 'NONE', *, *, #2103, .T. ) ;
#4280 = CARTESIAN_POINT ( 'NONE',  ( -60.99999999999998579, 14.72916666666666607, 2.077350269189628840 ) ) ;
#4281 = EDGE_CURVE ( 'NONE', #470, #5639, #133, .T. ) ;
#4282 = CARTESIAN_POINT ( 'NONE',  ( -62.86468353124999453, 9.015624999658601979, 1.500000000000002220 ) ) ;
#4283 = CARTESIAN_POINT ( 'NONE',  ( -61.99999999999998579, 13.65624999931720218, 2.654700538379254571 ) ) ;
#4284 = DIRECTION ( 'NONE',  ( 0.000000000000000000, -1.000000000000000000, 0.000000000000000000 ) ) ;
#4285 = ORIENTED_EDGE ( 'NONE', *, *, #4412, .F. ) ;
#4286 = TOROIDAL_SURFACE ( 'NONE', #8037, 1.336466033005844434, 0.5999999999999999778 ) ;
#4287 = CARTESIAN_POINT ( 'NONE',  ( -61.73205080756886076, 9.698664549684629321, 2.500000000000003109 ) ) ;
#4288 = CARTESIAN_POINT ( 'NONE',  ( -61.56765823437498142, 11.61979166632526805, 0.7511620957034663704 ) ) ;
#4289 = PRESENTATION_STYLE_ASSIGNMENT (( #2580 ) ) ;
#4290 =( BOUNDED_CURVE ( )  B_SPLINE_CURVE ( 2, ( #8591, #971, #7876, #7097, #1982, #7989, #196, #374, #257 ),
 .UNSPECIFIED., .F., .F. ) 
 B_SPLINE_CURVE_WITH_KNOTS ( ( 3, 2, 2, 2, 3 ),
 ( 0.7265625000000000000, 0.7291666666666666297, 0.7343750000000000000, 0.7395833333333333703, 0.7421875000000000000 ),
 .UNSPECIFIED. ) 
 CURVE ( )  GEOMETRIC_REPRESENTATION_ITEM ( )  RATIONAL_B_SPLINE_CURVE ( ( 0.9330127018922194093, 0.9330127018922194093, 1.000000000000000000, 0.8660254037844387076, 1.000000000000000000, 0.8660254037844387076, 1.000000000000000000, 0.9330127018922194093, 0.9330127018922194093 ) ) 
 REPRESENTATION_ITEM ( '' )  );
#4291 = CARTESIAN_POINT ( 'NONE',  ( -61.99999999999998579, 11.53124999931720218, 0.5000000000000013323 ) ) ;
#4292 = VERTEX_POINT ( 'NONE', #1077 ) ;
#4293 = CARTESIAN_POINT ( 'NONE',  ( -120.0000000000000000, -15.00000000000001421, 0.000000000000000000 ) ) ;
#4294 = CARTESIAN_POINT ( 'NONE',  ( -61.13531646874998415, 13.36979166632526628, 1.999225269531026417 ) ) ;
#4295 = CARTESIAN_POINT ( 'NONE',  ( -60.99999999999998579, 11.46874999931720218, 1.500000000000002220 ) ) ;
#4296 = CARTESIAN_POINT ( 'NONE',  ( -61.99999999999998579, 9.906249999317203958, 2.654700538379254571 ) ) ;
#4297 = ORIENTED_EDGE ( 'NONE', *, *, #497, .T. ) ;
#4298 = PRODUCT_DEFINITION_SHAPE ( 'NONE', 'NONE',  #10987 ) ;
#4299 = FACE_BOUND ( 'NONE', #738, .T. ) ;
#4300 = ORIENTED_EDGE ( 'NONE', *, *, #2587, .F. ) ;
#4301 = AXIS2_PLACEMENT_3D ( 'NONE', #3071, #573, #7129 ) ;
#4302 = DIRECTION ( 'NONE',  ( -0.000000000000000000, -0.000000000000000000, 1.000000000000000000 ) ) ;
#4303 = CARTESIAN_POINT ( 'NONE',  ( -61.13531646874998415, 11.09895833299193413, 1.000774730468978468 ) ) ;
#4304 = EDGE_CURVE ( 'NONE', #7871, #4292, #10235, .T. ) ;
#4305 = VERTEX_POINT ( 'NONE', #7870 ) ;
#4306 = CARTESIAN_POINT ( 'NONE',  ( -62.43234176562498305, 9.473958332991935904, 0.7511620957034662593 ) ) ;
#4307 = CARTESIAN_POINT ( 'NONE',  ( -61.99999999999998579, 13.90624999931720218, 2.500000000000002665 ) ) ;
#4308 = AXIS2_PLACEMENT_3D ( 'NONE', #8589, #859, #4875 ) ;
#4309 = CARTESIAN_POINT ( 'NONE',  ( -61.99999999999998579, 13.20312499965860198, 0.5015494609379544944 ) ) ;
#4310 = CARTESIAN_POINT ( 'NONE',  ( -60.99999999999998579, 8.239583332650536107, 0.9226497308103762673 ) ) ;
#4311 = VERTEX_POINT ( 'NONE', #4291 ) ;
#4312 = LINE ( 'NONE', #1829, #8513 ) ;
#4313 = ORIENTED_EDGE ( 'NONE', *, *, #2354, .F. ) ;
#4314 = CARTESIAN_POINT ( 'NONE',  ( -61.49999999999998579, 14.26041666598387003, 0.6339745962155628467 ) ) ;
#4315 = CARTESIAN_POINT ( 'NONE',  ( -61.13531646874998415, 14.84895833299193413, 1.000774730468978468 ) ) ;
#4316 = CARTESIAN_POINT ( 'NONE',  ( -62.99999999999998579, 8.864583332650536107, 2.077350269189627952 ) ) ;
#4317 = CARTESIAN_POINT ( 'NONE',  ( -61.99999999999998579, 16.00000000000000000, 0.5000000000000041078 ) ) ;
#4318 = DIRECTION ( 'NONE',  ( 0.000000000000000000, -0.000000000000000000, 1.000000000000000000 ) ) ;
#4319 = CARTESIAN_POINT ( 'NONE',  ( -61.99999999999999289, 14.20312499965860198, 0.5015494609379544944 ) ) ;
#4320 = EDGE_CURVE ( 'NONE', #5874, #10397, #2192, .T. ) ;
#4321 = CARTESIAN_POINT ( 'NONE',  ( -62.43234176562499016, 8.744791666325268054, 2.248837904296538071 ) ) ;
#4322 = CARTESIAN_POINT ( 'NONE',  ( -61.99999999999998579, 15.06249999999999822, 0.5000000000000013323 ) ) ;
#4323 = LINE ( 'NONE', #1842, #7979 ) ;
#4324 = CARTESIAN_POINT ( 'NONE',  ( -62.43234176562498305, 9.473958332991935904, 0.7511620957034662593 ) ) ;
#4325 = CARTESIAN_POINT ( 'NONE',  ( 0.3608130681495591019, 0.2499999999999982792, -1.888070236890895703 ) ) ;
#4326 = ORIENTED_EDGE ( 'NONE', *, *, #4701, .T. ) ;
#4327 = DIRECTION ( 'NONE',  ( -0.000000000000000000, -0.000000000000000000, -1.000000000000000000 ) ) ;
#4328 = CARTESIAN_POINT ( 'NONE',  ( -61.99999999999998579, 12.90624999931720218, 2.500000000000002665 ) ) ;
#4329 = CARTESIAN_POINT ( 'NONE',  ( -61.13531646874997705, 15.80729166632526628, 1.999225269531026417 ) ) ;
#4330 = CARTESIAN_POINT ( 'NONE',  ( -61.13531646874998415, 10.59895833299193413, 1.000774730468978468 ) ) ;
#4331 = CARTESIAN_POINT ( 'NONE',  ( -61.99999999999999289, 9.515624999658600203, 2.498450539062049724 ) ) ;
#4332 = ORIENTED_EDGE ( 'NONE', *, *, #9866, .T. ) ;
#4333 = CARTESIAN_POINT ( 'NONE',  ( -60.99999999999998579, 15.72916666666666785, 2.077350269189628840 ) ) ;
#4334 = CARTESIAN_POINT ( 'NONE',  ( -62.43234176562498305, 10.72395833299193413, 0.7511620957034662593 ) ) ;
#4335 = DIRECTION ( 'NONE',  ( 1.000000000000000000, 0.000000000000000000, 0.000000000000000000 ) ) ;
#4336 = CARTESIAN_POINT ( 'NONE',  ( -61.49999999999998579, 12.92708333265053611, 2.366025403784441927 ) ) ;
#4337 = CARTESIAN_POINT ( 'NONE',  ( 0.000000000000000000, 0.000000000000000000, 0.000000000000000000 ) ) ;
#4338 = ORIENTED_EDGE ( 'NONE', *, *, #6256, .T. ) ;
#4339 = DIRECTION ( 'NONE',  ( 0.000000000000000000, 1.000000000000000000, 0.000000000000000000 ) ) ;
#4340 = CARTESIAN_POINT ( 'NONE',  ( -62.86468353124999453, 11.95312499965860198, 1.500000000000002220 ) ) ;
#4341 = FACE_OUTER_BOUND ( 'NONE', #986, .T. ) ;
#4342 = CARTESIAN_POINT ( 'NONE',  ( -61.73205080756886076, 15.44866454968462932, 2.500000000000003109 ) ) ;
#4343 = EDGE_LOOP ( 'NONE', ( #2549, #2488 ) ) ;
#4344 = CARTESIAN_POINT ( 'NONE',  ( -57.99999999999998579, -14.00000000000001243, 0.000000000000000000 ) ) ;
#4345 = CARTESIAN_POINT ( 'NONE',  ( -61.99999999999998579, 12.70312499965860198, 0.5015494609379544944 ) ) ;
#4346 =( LENGTH_UNIT ( ) NAMED_UNIT ( * ) SI_UNIT ( .MILLI., .METRE. ) );
#4347 = CARTESIAN_POINT ( 'NONE',  ( -49.99999999999998579, 3.999999999999980904, 0.000000000000000000 ) ) ;
#4348 = CARTESIAN_POINT ( 'NONE',  ( -62.49999999999998579, 8.635416665983868256, 2.366025403784441483 ) ) ;
#4349 = ORIENTED_EDGE ( 'NONE', *, *, #9274, .T. ) ;
#4350 = DIRECTION ( 'NONE',  ( 0.000000000000000000, -0.000000000000000000, 1.000000000000000000 ) ) ;
#4351 = CARTESIAN_POINT ( 'NONE',  ( -49.99999999999998579, -15.00000000000001066, 3.000000000000000000 ) ) ;
#4352 = EDGE_CURVE ( 'NONE', #8495, #7998, #5985, .T. ) ;
#4353 =( BOUNDED_CURVE ( )  B_SPLINE_CURVE ( 2, ( #3781, #8956, #6400, #4715, #9553, #8123, #9724, #9786, #5556 ),
 .UNSPECIFIED., .F., .T. ) 
 B_SPLINE_CURVE_WITH_KNOTS ( ( 3, 2, 2, 2, 3 ),
 ( 0.4921875000000000000, 0.4947916666666666852, 0.5000000000000000000, 0.5052083333333333703, 0.5078125000000000000 ),
 .UNSPECIFIED. ) 
 CURVE ( )  GEOMETRIC_REPRESENTATION_ITEM ( )  RATIONAL_B_SPLINE_CURVE ( ( 0.9330127018922194093, 0.9330127018922194093, 1.000000000000000000, 0.8660254037844387076, 1.000000000000000000, 0.8660254037844387076, 1.000000000000000000, 0.9330127018922194093, 0.9330127018922194093 ) ) 
 REPRESENTATION_ITEM ( '' )  );
#4354 = CARTESIAN_POINT ( 'NONE',  ( -62.86468353124998032, 11.18229166632526983, 1.000774730468978246 ) ) ;
#4355 = ORIENTED_EDGE ( 'NONE', *, *, #4171, .F. ) ;
#4356 = CARTESIAN_POINT ( 'NONE',  ( -62.43234176562499016, 9.307291666325268054, 2.248837904296538071 ) ) ;
#4357 = DIRECTION ( 'NONE',  ( -0.000000000000000000, -0.000000000000000000, -1.000000000000000000 ) ) ;
#4358 = CARTESIAN_POINT ( 'NONE',  ( -62.86468353124999453, 15.01562499965860020, 1.500000000000002220 ) ) ;
#4359 = EDGE_CURVE ( 'NONE', #3891, #5034, #7313, .T. ) ;
#4360 = CARTESIAN_POINT ( 'NONE',  ( 150.0000000000000000, 8.000000000000000000, 0.000000000000000000 ) ) ;
#4361 = VERTEX_POINT ( 'NONE', #430 ) ;
#4363 = EDGE_CURVE ( 'NONE', #4192, #1707, #2930, .T. ) ;
#4362 = DIRECTION ( 'NONE',  ( 1.000000000000000000, 0.000000000000000000, 0.000000000000000000 ) ) ;
#4364 = PRESENTATION_LAYER_ASSIGNMENT (  '', '', ( #6538 ) ) ;
#4365 = ORIENTED_EDGE ( 'NONE', *, *, #2100, .F. ) ;
#4366 = CARTESIAN_POINT ( 'NONE',  ( -61.99999999999998579, 14.99999999999998579, 0.5000000000000013323 ) ) ;
#4367 = CARTESIAN_POINT ( 'NONE',  ( -61.99999999999998579, 8.562500000000001776, 0.3452994616207497591 ) ) ;
#4368 = CARTESIAN_POINT ( 'NONE',  ( -62.26794919243111082, 9.823664549684629321, 0.5000000000000013323 ) ) ;
#4369 = CARTESIAN_POINT ( 'NONE',  ( 140.0000000000000284, -8.000000000000000000, 4.000000000000000000 ) ) ;
#4370 = FACE_OUTER_BOUND ( 'NONE', #6426, .T. ) ;
#4371 = ADVANCED_FACE ( 'NONE', ( #1320 ), #2870, .F. ) ;
#4372 = CARTESIAN_POINT ( 'NONE',  ( -62.86468353124999453, 14.28645833299193413, 1.999225269531025750 ) ) ;
#4373 = CARTESIAN_POINT ( 'NONE',  ( -61.99999999999998579, 9.390624999658600203, 0.5015494609379544944 ) ) ;
#4374 = LINE ( 'NONE', #457, #6002 ) ;
#4375 = CARTESIAN_POINT ( 'NONE',  ( -62.26794919243111082, 15.79241454900183506, 0.5000000000000013323 ) ) ;
#4376 = CARTESIAN_POINT ( 'NONE',  ( -62.43234176562499016, 8.557291666325268054, 2.248837904296538071 ) ) ;
#4377 = EDGE_CURVE ( 'NONE', #8566, #7983, #10470, .T. ) ;
#4378 = CARTESIAN_POINT ( 'NONE',  ( -62.26794919243111082, 14.14508544963257286, 2.500000000000003109 ) ) ;
#4379 = ORIENTED_EDGE ( 'NONE', *, *, #4633, .F. ) ;
#4380 = LINE ( 'NONE', #3558, #8498 ) ;
#4381 = CARTESIAN_POINT ( 'NONE',  ( -61.49999999999998579, 11.26041666598387003, 0.6339745962155628467 ) ) ;
#4382 = EDGE_CURVE ( 'NONE', #5639, #2471, #5465, .T. ) ;
#4383 = CARTESIAN_POINT ( 'NONE',  ( -62.86468353124999453, 14.95312499965860020, 1.500000000000002220 ) ) ;
#4384 = CARTESIAN_POINT ( 'NONE',  ( -62.86468353124998032, 11.43229166632526805, 1.000774730468978246 ) ) ;
#4385 = VECTOR ( 'NONE', #7671, 1000.000000000000000 ) ;
#4386 = CARTESIAN_POINT ( 'NONE',  ( -61.13531646874997705, 9.098958332991935904, 1.000774730468978468 ) ) ;
#4387 = CARTESIAN_POINT ( 'NONE',  ( -60.99999999999998579, 9.697916665983870033, 2.077350269189628840 ) ) ;
#4388 = EDGE_LOOP ( 'NONE', ( #4659, #4228, #5013, #651, #128, #502, #8779, #5188 ) ) ;
#4389 = CARTESIAN_POINT ( 'NONE',  ( -61.49999999999998579, 15.04166666666666607, 0.6339745962155628467 ) ) ;
#4390 = CARTESIAN_POINT ( 'NONE',  ( -61.13531646874998415, 10.14062499965860198, 1.500000000000002220 ) ) ;
#4391 = CARTESIAN_POINT ( 'NONE',  ( 0.000000000000000000, 0.000000000000000000, 0.000000000000000000 ) ) ;
#4392 = CARTESIAN_POINT ( 'NONE',  ( -61.99999999999998579, 13.15624999931720396, 2.654700538379254571 ) ) ;
#4393 = CARTESIAN_POINT ( 'NONE',  ( -49.99999999999998579, 2.500000000000000444, 83.15773105863907233 ) ) ;
#4394 = ORIENTED_EDGE ( 'NONE', *, *, #146, .T. ) ;
#4395 = CARTESIAN_POINT ( 'NONE',  ( -61.99999999999998579, 16.00000000000000000, 1.500000000000002220 ) ) ;
#4396 = AXIS2_PLACEMENT_3D ( 'NONE', #4668, #4825, #8181 ) ;
#4397 = EDGE_CURVE ( 'NONE', #9156, #7362, #9253, .T. ) ;
#4398 = AXIS2_PLACEMENT_3D ( 'NONE', #5923, #5809, #10870 ) ;
#4399 = CARTESIAN_POINT ( 'NONE',  ( -61.99999999999999289, 11.64062499965860198, 0.5015494609379544944 ) ) ;
#4400 = CARTESIAN_POINT ( 'NONE',  ( -62.99999999999998579, 15.64583333333333393, 2.077350269189627952 ) ) ;
#4401 = APPLICATION_CONTEXT ( 'automotive_design' ) ;
#4402 = CARTESIAN_POINT ( 'NONE',  ( -61.49999999999998579, 13.04166666666666607, 0.6339745962155628467 ) ) ;
#4403 = ORIENTED_EDGE ( 'NONE', *, *, #10665, .T. ) ;
#4404 = CARTESIAN_POINT ( 'NONE',  ( -62.49999999999998579, 10.91666666666666607, 2.366025403784441483 ) ) ;
#4405 = CARTESIAN_POINT ( 'NONE',  ( -61.99999999999998579, 16.00000000000000000, 1.500000000000002220 ) ) ;
#4406 = AXIS2_PLACEMENT_3D ( 'NONE', #9845, #568, #7232 ) ;
#4407 = CARTESIAN_POINT ( 'NONE',  ( -61.99999999999998579, 13.70312499965860198, 0.5015494609379544944 ) ) ;
#4408 =( LENGTH_UNIT ( ) NAMED_UNIT ( * ) SI_UNIT ( .MILLI., .METRE. ) );
#4409 = CARTESIAN_POINT ( 'NONE',  ( -61.49999999999998579, 10.20833333333333393, 2.366025403784441927 ) ) ;
#4410 = CARTESIAN_POINT ( 'NONE',  ( -62.49999999999998579, 9.385416665983870033, 2.366025403784441483 ) ) ;
#4411 = PRESENTATION_LAYER_ASSIGNMENT (  '', '', ( #4234 ) ) ;
#4412 = EDGE_CURVE ( 'NONE', #5522, #3958, #7146, .T. ) ;
#4413 = VERTEX_POINT ( 'NONE', #8204 ) ;
#4414 = LINE ( 'NONE', #5357, #4071 ) ;
#4415 = CARTESIAN_POINT ( 'NONE',  ( -60.99999999999998579, 9.968749999317202182, 1.500000000000002220 ) ) ;
#4416 = VECTOR ( 'NONE', #6796, 1000.000000000000000 ) ;
#4417 = EDGE_CURVE ( 'NONE', #9464, #35, #6297, .T. ) ;
#4418 = CARTESIAN_POINT ( 'NONE',  ( -61.56765823437498142, 10.86979166632526805, 0.7511620957034663704 ) ) ;
#4419 = FILL_AREA_STYLE ('',( #4249 ) ) ;
#4420 = ORIENTED_EDGE ( 'NONE', *, *, #1732, .T. ) ;
#4421 = CARTESIAN_POINT ( 'NONE',  ( -61.13531646874998415, 10.39062499965860198, 1.500000000000002220 ) ) ;
#4422 = DIRECTION ( 'NONE',  ( 0.000000000000000000, 1.000000000000000000, 0.000000000000000000 ) ) ;
#4423 = EDGE_CURVE ( 'NONE', #7302, #2222, #6769, .T. ) ;
#4424 = VECTOR ( 'NONE', #8004, 1000.000000000000000 ) ;
#4425 = CARTESIAN_POINT ( 'NONE',  ( -61.99999999999998579, 14.07812499965860020, 2.498450539062049724 ) ) ;
#4426 = AXIS2_PLACEMENT_3D ( 'NONE', #3626, #5337, #7915 ) ;
#4427 = CARTESIAN_POINT ( 'NONE',  ( -62.99999999999998579, 12.07291666598387181, 0.9226497308103756012 ) ) ;
#4428 = ORIENTED_EDGE ( 'NONE', *, *, #7372, .T. ) ;
#4429 =( BOUNDED_CURVE ( )  B_SPLINE_CURVE ( 2, ( #2821, #6210, #6094, #10366, #5301, #4476, #5535, #9823, #1378 ),
 .UNSPECIFIED., .F., .T. ) 
 B_SPLINE_CURVE_WITH_KNOTS ( ( 3, 2, 2, 2, 3 ),
 ( 0.6640625000000000000, 0.6666666666666666297, 0.6718750000000000000, 0.6770833333333333703, 0.6796875000000000000 ),
 .UNSPECIFIED. ) 
 CURVE ( )  GEOMETRIC_REPRESENTATION_ITEM ( )  RATIONAL_B_SPLINE_CURVE ( ( 0.9330127018922194093, 0.9330127018922194093, 1.000000000000000000, 0.8660254037844387076, 1.000000000000000000, 0.8660254037844387076, 1.000000000000000000, 0.9330127018922194093, 0.9330127018922194093 ) ) 
 REPRESENTATION_ITEM ( '' )  );
#4430 = CARTESIAN_POINT ( 'NONE',  ( -61.99999999999998579, 10.56249999999999822, 0.5000000000000013323 ) ) ;
#4431 = ORIENTED_EDGE ( 'NONE', *, *, #5763, .F. ) ;
#4432 = CARTESIAN_POINT ( 'NONE',  ( -60.99999999999998579, 12.73958333265053611, 0.9226497308103762673 ) ) ;
#4433 = CARTESIAN_POINT ( 'NONE',  ( -61.99999999999998579, 8.312500000000000000, 0.3452994616207497591 ) ) ;
#4434 = CARTESIAN_POINT ( 'NONE',  ( -62.99999999999998579, 8.822916665983868256, 0.9226497308103756012 ) ) ;
#4435 = CARTESIAN_POINT ( 'NONE',  ( -114.9999999999999289, -7.999999999999998224, -2.000000000000000000 ) ) ;
#4436 = LINE ( 'NONE', #5497, #7776 ) ;
#4437 = CARTESIAN_POINT ( 'NONE',  ( -62.43234176562499016, 13.80729166632526805, 2.248837904296538071 ) ) ;
#4438 = CARTESIAN_POINT ( 'NONE',  ( -61.56765823437498142, 8.619791666325268054, 0.7511620957034663704 ) ) ;
#4439 = CARTESIAN_POINT ( 'NONE',  ( -61.73205080756886787, 9.198664549684631098, 2.500000000000004885 ) ) ;
#4440 = DIRECTION ( 'NONE',  ( 1.000000000000000000, -0.000000000000000000, -0.000000000000000000 ) ) ;
#4441 = CARTESIAN_POINT ( 'NONE',  ( -61.99999999999998579, 10.45312499965860198, 0.5015494609379544944 ) ) ;
#4442 = DIRECTION ( 'NONE',  ( 1.000000000000000000, 0.000000000000000000, 0.000000000000000000 ) ) ;
#4443 = ORIENTED_EDGE ( 'NONE', *, *, #7358, .T. ) ;
#4444 = DIRECTION ( 'NONE',  ( 0.000000000000000000, -0.000000000000000000, -1.000000000000000000 ) ) ;
#4445 = CARTESIAN_POINT ( 'NONE',  ( -60.99999999999998579, 12.96874999931720396, 1.500000000000002220 ) ) ;
#4446 = EDGE_CURVE ( 'NONE', #9263, #7983, #6259, .T. ) ;
#4447 = DIRECTION ( 'NONE',  ( -0.000000000000000000, -1.000000000000000000, -0.000000000000000000 ) ) ;
#4448 = CARTESIAN_POINT ( 'NONE',  ( -62.86468353124998742, 12.47395833299193413, 1.999225269531025972 ) ) ;
#4449 = EDGE_CURVE ( 'NONE', #6224, #6875, #9645, .T. ) ;
#4450 = CARTESIAN_POINT ( 'NONE',  ( -62.43234176562499016, 9.244791666325268054, 2.248837904296538071 ) ) ;
#4451 = CARTESIAN_POINT ( 'NONE',  ( -60.99999999999998579, 9.718749999317202182, 1.500000000000002220 ) ) ;
#4452 = VERTEX_POINT ( 'NONE', #1196 ) ;
#4453 = CARTESIAN_POINT ( 'NONE',  ( -62.49999999999998579, 10.80208333265053611, 0.6339745962155627357 ) ) ;
#4454 = VECTOR ( 'NONE', #10396, 1000.000000000000000 ) ;
#4455 = CARTESIAN_POINT ( 'NONE',  ( -61.99999999999999289, 9.453124999658600203, 0.5015494609379544944 ) ) ;
#4456 = DIRECTION ( 'NONE',  ( 0.000000000000000000, 0.000000000000000000, 1.000000000000000000 ) ) ;
#4457 = CARTESIAN_POINT ( 'NONE',  ( -61.13531646874998415, 15.82812499965860198, 1.500000000000002220 ) ) ;
#4458 = CARTESIAN_POINT ( 'NONE',  ( -60.99999999999998579, 14.94791666598387003, 2.077350269189628840 ) ) ;
#4459 = CARTESIAN_POINT ( 'NONE',  ( -61.99999999999998579, 13.18750000000000000, 2.500000000000002665 ) ) ;
#4460 = ORIENTED_EDGE ( 'NONE', *, *, #1987, .T. ) ;
#4461 = LINE ( 'NONE', #2749, #10525 ) ;
#4462 = AXIS2_PLACEMENT_3D ( 'NONE', #8254, #2349, #3135 ) ;
#4463 = CARTESIAN_POINT ( 'NONE',  ( -62.86468353124998032, 11.93229166632526628, 1.000774730468978024 ) ) ;
#4464 = CARTESIAN_POINT ( 'NONE',  ( -62.86468353124998032, 9.182291666325268054, 1.000774730468978246 ) ) ;
#4465 = DIRECTION ( 'NONE',  ( 0.000000000000000000, 0.000000000000000000, 1.000000000000000000 ) ) ;
#4466 = VERTEX_POINT ( 'NONE', #4576 ) ;
#4467 = CARTESIAN_POINT ( 'NONE',  ( -62.99999999999998579, 10.85416666666666785, 0.9226497308103756012 ) ) ;
#4468 = DIRECTION ( 'NONE',  ( 0.000000000000000000, 1.000000000000000000, 0.000000000000000000 ) ) ;
#4469 = CARTESIAN_POINT ( 'NONE',  ( -61.99999999999998579, 14.07812499965860020, 2.498450539062049724 ) ) ;
#4470 = DIRECTION ( 'NONE',  ( 1.000000000000000000, 0.000000000000000000, 0.000000000000000000 ) ) ;
#4471 = EDGE_CURVE ( 'NONE', #6004, #5909, #3040, .T. ) ;
#4472 = VECTOR ( 'NONE', #4007, 1000.000000000000000 ) ;
#4473 = CARTESIAN_POINT ( 'NONE',  ( -61.99999999999998579, 8.781249999317203958, 0.3452994616207497591 ) ) ;
#4474 = EDGE_LOOP ( 'NONE', ( #4016, #3685, #8431, #2170 ) ) ;
#4475 = DIRECTION ( 'NONE',  ( -1.000000000000000000, -0.000000000000000000, -0.000000000000000000 ) ) ;
#4476 = CARTESIAN_POINT ( 'NONE',  ( -62.99999999999998579, 13.39583333333333393, 2.077350269189627952 ) ) ;
#4477 = VECTOR ( 'NONE', #6427, 1000.000000000000000 ) ;
#4478 = CARTESIAN_POINT ( 'NONE',  ( -62.43234176562499016, 10.99479166632526805, 2.248837904296538071 ) ) ;
#4479 = VECTOR ( 'NONE', #1917, 1000.000000000000000 ) ;
#4480 = EDGE_LOOP ( 'NONE', ( #6392, #5597, #10932, #8542, #450, #8676, #5228, #8441 ) ) ;
#4481 = CARTESIAN_POINT ( 'NONE',  ( -61.56765823437498852, 9.848958332991934128, 2.248837904296538515 ) ) ;
#4482 = CARTESIAN_POINT ( 'NONE',  ( -62.99999999999998579, 15.61458333265053433, 2.077350269189627952 ) ) ;
#4483 = CARTESIAN_POINT ( 'NONE',  ( -62.86468353124998032, 14.74479166632526628, 1.000774730468978246 ) ) ;
#4484 = CARTESIAN_POINT ( 'NONE',  ( -61.99999999999998579, 11.18750000000000000, 2.500000000000002665 ) ) ;
#4485 = EDGE_LOOP ( 'NONE', ( #9563, #361, #3244, #3136 ) ) ;
#4486 = CARTESIAN_POINT ( 'NONE',  ( 0.04978537780227577231, -0.2499999999999997224, -1.594765474869573874 ) ) ;
#4487 = ADVANCED_FACE ( 'NONE', ( #4745 ), #6488, .F. ) ;
#4488 = EDGE_LOOP ( 'NONE', ( #4156, #7221 ) ) ;
#4489 = FACE_OUTER_BOUND ( 'NONE', #9665, .T. ) ;
#4490 = CARTESIAN_POINT ( 'NONE',  ( -61.49999999999998579, 8.791666666666666075, 0.6339745962155628467 ) ) ;
#4491 = FACE_OUTER_BOUND ( 'NONE', #5816, .T. ) ;
#4492 = CARTESIAN_POINT ( 'NONE',  ( 145.0000000000000284, 5.500000000000000000, 6.000000000000000000 ) ) ;
#4493 = DIRECTION ( 'NONE',  ( 0.000000000000000000, 0.000000000000000000, 1.000000000000000000 ) ) ;
#4494 = CARTESIAN_POINT ( 'NONE',  ( -62.86468353124998032, 13.74479166632526805, 1.000774730468978024 ) ) ;
#4495 = CARTESIAN_POINT ( 'NONE',  ( -61.99999999999998579, 9.515624999658601979, 2.498450539062049724 ) ) ;
#4496 = CARTESIAN_POINT ( 'NONE',  ( -61.99999999999997868, 11.28124999931720041, 0.5000000000000013323 ) ) ;
#4497 =( BOUNDED_CURVE ( )  B_SPLINE_CURVE ( 2, ( #10631, #681, #3030, #4065, #3133, #1365, #3230, #6530, #9912 ),
 .UNSPECIFIED., .F., .T. ) 
 B_SPLINE_CURVE_WITH_KNOTS ( ( 3, 2, 2, 2, 3 ),
 ( 0.8828125000000000000, 0.8854166666666666297, 0.8906250000000000000, 0.8958333333333333703, 0.8984375000000000000 ),
 .UNSPECIFIED. ) 
 CURVE ( )  GEOMETRIC_REPRESENTATION_ITEM ( )  RATIONAL_B_SPLINE_CURVE ( ( 0.9330127018922194093, 0.9330127018922194093, 1.000000000000000000, 0.8660254037844387076, 1.000000000000000000, 0.8660254037844387076, 1.000000000000000000, 0.9330127018922194093, 0.9330127018922194093 ) ) 
 REPRESENTATION_ITEM ( '' )  );
#4498 = DIRECTION ( 'NONE',  ( 0.000000000000000000, 1.000000000000000000, 0.000000000000000000 ) ) ;
#4499 = CARTESIAN_POINT ( 'NONE',  ( -61.13531646874998415, 10.14062499965860198, 1.500000000000002220 ) ) ;
#4500 = DIRECTION ( 'NONE',  ( 1.000000000000000000, 0.000000000000000000, 0.000000000000000000 ) ) ;
#4501 = ORIENTED_EDGE ( 'NONE', *, *, #6269, .F. ) ;
#4502 = CARTESIAN_POINT ( 'NONE',  ( -105.0000000000000000, -2.500000000000000000, 4.000000000000000000 ) ) ;
#4503 = CARTESIAN_POINT ( 'NONE',  ( -61.99999999999997868, 11.43750000000000000, 2.500000000000002665 ) ) ;
#4504 = EDGE_CURVE ( 'NONE', #1211, #5256, #7334, .T. ) ;
#4505 = CARTESIAN_POINT ( 'NONE',  ( -57.99999999999998579, -10.00000000000000888, 3.000000000000000000 ) ) ;
#4506 = CARTESIAN_POINT ( 'NONE',  ( -61.99999999999998579, 12.76562499965860198, 2.498450539062049724 ) ) ;
#4507 = CARTESIAN_POINT ( 'NONE',  ( -62.43234176562499016, 8.744791666325268054, 2.248837904296538071 ) ) ;
#4508 = DIRECTION ( 'NONE',  ( -0.000000000000000000, -0.000000000000000000, 1.000000000000000000 ) ) ;
#4509 = VERTEX_POINT ( 'NONE', #7527 ) ;
#4510 = CARTESIAN_POINT ( 'NONE',  ( -61.99999999999998579, 10.78124999931720218, 0.5000000000000013323 ) ) ;
#4511 = CARTESIAN_POINT ( 'NONE',  ( -62.43234176562498305, 9.973958332991934128, 0.7511620957034662593 ) ) ;
#4512 = DIRECTION ( 'NONE',  ( 1.000000000000000000, 0.000000000000000000, 0.000000000000000000 ) ) ;
#4513 = CARTESIAN_POINT ( 'NONE',  ( -62.43234176562499016, 14.99479166632526805, 2.248837904296538071 ) ) ;
#4514 = CARTESIAN_POINT ( 'NONE',  ( -61.49999999999998579, 14.17708333265053611, 2.366025403784441927 ) ) ;
#4515 = DIRECTION ( 'NONE',  ( 0.000000000000000000, 0.000000000000000000, 1.000000000000000000 ) ) ;
#4516 = ORIENTED_EDGE ( 'NONE', *, *, #5254, .F. ) ;
#4517 = CARTESIAN_POINT ( 'NONE',  ( 145.0000000000000284, -5.500000000000000000, 3.000000000000000000 ) ) ;
#4518 = EDGE_LOOP ( 'NONE', ( #8155, #8199, #1817, #5806 ) ) ;
#4519 = ADVANCED_FACE ( 'NONE', ( #4076 ), #9140, .T. ) ;
#4520 = CARTESIAN_POINT ( 'NONE',  ( -62.86468353124999453, 12.45312499965860198, 1.500000000000002220 ) ) ;
#4521 = DIRECTION ( 'NONE',  ( 0.000000000000000000, 0.000000000000000000, -1.000000000000000000 ) ) ;
#4522 = LINE ( 'NONE', #5234, #4479 ) ;
#4523 = ORIENTED_EDGE ( 'NONE', *, *, #5916, .F. ) ;
#4524 = CARTESIAN_POINT ( 'NONE',  ( -62.99999999999998579, 12.62500000000000000, 1.500000000000001998 ) ) ;
#4525 = CYLINDRICAL_SURFACE ( 'NONE', #8560, 0.9999999999999981126 ) ;
#4526 = CARTESIAN_POINT ( 'NONE',  ( -61.13531646874998415, 14.91145833299193413, 1.000774730468978468 ) ) ;
#4527 = CARTESIAN_POINT ( 'NONE',  ( -31.99999999999998579, -14.00000000000000888, 5.000000000000000000 ) ) ;
#4528 = CARTESIAN_POINT ( 'NONE',  ( -62.99999999999998579, 10.61458333265053611, 2.077350269189627952 ) ) ;
#4529 = ORIENTED_EDGE ( 'NONE', *, *, #4281, .F. ) ;
#4530 = DIRECTION ( 'NONE',  ( 0.000000000000000000, 0.000000000000000000, 1.000000000000000000 ) ) ;
#4531 = LINE ( 'NONE', #1874, #7763 ) ;
#4532 = CARTESIAN_POINT ( 'NONE',  ( -61.99999999999998579, 11.26562499965860198, 2.498450539062049724 ) ) ;
#4533 = EDGE_CURVE ( 'NONE', #2384, #5580, #6656, .T. ) ;
#4534 = ORIENTED_EDGE ( 'NONE', *, *, #4812, .T. ) ;
#4535 = CARTESIAN_POINT ( 'NONE',  ( -61.99999999999998579, 10.07812499965860198, 2.498450539062049724 ) ) ;
#4536 = CARTESIAN_POINT ( 'NONE',  ( -149.9999999999999716, -12.99999999999998757, 3.000000000000000000 ) ) ;
#4537 = CARTESIAN_POINT ( 'NONE',  ( -62.86468353124998032, 14.49479166632526805, 1.000774730468978246 ) ) ;
#4538 = CARTESIAN_POINT ( 'NONE',  ( -99.99999999999998579, 15.67949192431120053, 0.000000000000000000 ) ) ;
#4539 = VERTEX_POINT ( 'NONE', #8260 ) ;
#4540 = CARTESIAN_POINT ( 'NONE',  ( -49.99999999999998579, -8.000000000000000000, 3.000000000000000000 ) ) ;
#4541 = VERTEX_POINT ( 'NONE', #5012 ) ;
#4542 = CARTESIAN_POINT ( 'NONE',  ( -62.99999999999998579, 15.07291666598387003, 0.9226497308103756012 ) ) ;
#4543 = CARTESIAN_POINT ( 'NONE',  ( -60.99999999999998579, 8.020833333333333925, 0.9226497308103762673 ) ) ;
#4544 = CARTESIAN_POINT ( 'NONE',  ( -120.0000000000000000, -15.00000000000001421, 83.15773105863907233 ) ) ;
#4545 = CARTESIAN_POINT ( 'NONE',  ( -61.99999999999998579, 16.15624999931720041, 2.500000000000002665 ) ) ;
#4546 = CYLINDRICAL_SURFACE ( 'NONE', #9922, 0.9999999999999981126 ) ;
#4547 = CARTESIAN_POINT ( 'NONE',  ( -61.56765823437498142, 14.68229166632526805, 0.7511620957034663704 ) ) ;
#4548 = CARTESIAN_POINT ( 'NONE',  ( -62.86468353124999453, 10.20312499965860198, 1.500000000000002220 ) ) ;
#4549 = DIRECTION ( 'NONE',  ( -0.000000000000000000, -0.000000000000000000, 1.000000000000000000 ) ) ;
#4550 = LINE ( 'NONE', #7957, #9752 ) ;
#4551 = CARTESIAN_POINT ( 'NONE',  ( -61.13531646874998415, 10.66145833299193413, 1.000774730468978468 ) ) ;
#4552 = CARTESIAN_POINT ( 'NONE',  ( -61.99999999999998579, 9.562500000000000000, 0.5000000000000013323 ) ) ;
#4553 = ORIENTED_EDGE ( 'NONE', *, *, #3905, .F. ) ;
#4554 = DIRECTION ( 'NONE',  ( -0.7071067811865463515, 0.000000000000000000, -0.7071067811865487940 ) ) ;
#4555 = ADVANCED_FACE ( 'NONE', ( #8303 ), #5693, .F. ) ;
#4556 = EDGE_LOOP ( 'NONE', ( #3077, #9544, #5564, #9901 ) ) ;
#4557 = CARTESIAN_POINT ( 'NONE',  ( -60.99999999999998579, 10.00000000000000000, 1.500000000000002220 ) ) ;
#4558 = CARTESIAN_POINT ( 'NONE',  ( -62.86468353124998742, 12.22395833299193413, 1.999225269531025972 ) ) ;
#4559 = CARTESIAN_POINT ( 'NONE',  ( -61.13531646874998415, 8.828124999658601979, 1.500000000000002220 ) ) ;
#4560 = CARTESIAN_POINT ( 'NONE',  ( -61.99999999999998579, 26.00000000000000355, 1.500000000000002220 ) ) ;
#4561 =( BOUNDED_CURVE ( )  B_SPLINE_CURVE ( 2, ( #987, #7668, #5043, #9435, #10156, #6048, #1834, #8393, #7612 ),
 .UNSPECIFIED., .F., .T. ) 
 B_SPLINE_CURVE_WITH_KNOTS ( ( 3, 2, 2, 2, 3 ),
 ( 0.6171875000000000000, 0.6197916666666666297, 0.6250000000000000000, 0.6302083333333333703, 0.6328125000000000000 ),
 .UNSPECIFIED. ) 
 CURVE ( )  GEOMETRIC_REPRESENTATION_ITEM ( )  RATIONAL_B_SPLINE_CURVE ( ( 0.9330127018922194093, 0.9330127018922194093, 1.000000000000000000, 0.8660254037844387076, 1.000000000000000000, 0.8660254037844387076, 1.000000000000000000, 0.9330127018922194093, 0.9330127018922194093 ) ) 
 REPRESENTATION_ITEM ( '' )  );
#4562 = ORIENTED_EDGE ( 'NONE', *, *, #10476, .F. ) ;
#4563 = DIRECTION ( 'NONE',  ( 0.000000000000000000, 0.000000000000000000, -1.000000000000000000 ) ) ;
#4564 = CARTESIAN_POINT ( 'NONE',  ( -62.86468353124998032, 9.994791666325268054, 1.000774730468978024 ) ) ;
#4565 = AXIS2_PLACEMENT_3D ( 'NONE', #8826, #1210, #4591 ) ;
#4566 = CARTESIAN_POINT ( 'NONE',  ( -61.56765823437498852, 15.78645833299193590, 2.248837904296538515 ) ) ;
#4567 = ADVANCED_FACE ( 'NONE', ( #2463, #6595, #6648 ), #4961, .F. ) ;
#4568 = CARTESIAN_POINT ( 'NONE',  ( -62.99999999999998579, 15.09374999931720218, 1.500000000000001998 ) ) ;
#4569 = CARTESIAN_POINT ( 'NONE',  ( -61.99999999999998579, 16.03124999931720041, 0.5000000000000013323 ) ) ;
#4570 = VERTEX_POINT ( 'NONE', #3345 ) ;
#4571 = FACE_OUTER_BOUND ( 'NONE', #1640, .T. ) ;
#4572 = ORIENTED_EDGE ( 'NONE', *, *, #7473, .F. ) ;
#4573 = CARTESIAN_POINT ( 'NONE',  ( -61.13531646874997705, 12.34895833299193413, 1.000774730468978468 ) ) ;
#4574 = CARTESIAN_POINT ( 'NONE',  ( -61.56765823437498852, 8.536458332991934128, 2.248837904296538515 ) ) ;
#4575 = AXIS2_PLACEMENT_3D ( 'NONE', #609, #3884, #7277 ) ;
#4576 = CARTESIAN_POINT ( 'NONE',  ( -109.9999999999999289, 33.00000000000000711, 0.000000000000000000 ) ) ;
#4577 = ORIENTED_EDGE ( 'NONE', *, *, #826, .F. ) ;
#4578 = CARTESIAN_POINT ( 'NONE',  ( -61.49999999999998579, 12.70833333333333393, 2.366025403784441927 ) ) ;
#4579 = FACE_OUTER_BOUND ( 'NONE', #3924, .T. ) ;
#4580 = CARTESIAN_POINT ( 'NONE',  ( -61.99999999999998579, 14.45312499965860020, 0.5015494609379544944 ) ) ;
#4581 =( NAMED_UNIT ( * ) PLANE_ANGLE_UNIT ( ) SI_UNIT ( $, .RADIAN. ) );
#4582 = CARTESIAN_POINT ( 'NONE',  ( 0.000000000000000000, 0.000000000000000000, 4.000000000000000000 ) ) ;
#4583 = VECTOR ( 'NONE', #275, 1000.000000000000000 ) ;
#4584 = CARTESIAN_POINT ( 'NONE',  ( -60.99999999999998579, 11.21874999931720218, 1.500000000000002220 ) ) ;
#4585 = VERTEX_POINT ( 'NONE', #6747 ) ;
#4586 = DIRECTION ( 'NONE',  ( 0.000000000000000000, 0.000000000000000000, -1.000000000000000000 ) ) ;
#4587 = VECTOR ( 'NONE', #7705, 1000.000000000000000 ) ;
#4588 = DIRECTION ( 'NONE',  ( 1.000000000000000000, 0.000000000000000000, 0.000000000000000000 ) ) ;
#4589 = CARTESIAN_POINT ( 'NONE',  ( -61.56765823437498142, 12.11979166632526628, 0.7511620957034663704 ) ) ;
#4590 = EDGE_CURVE ( 'NONE', #918, #8781, #9088, .T. ) ;
#4591 = DIRECTION ( 'NONE',  ( 1.000000000000000000, 0.000000000000000000, 0.000000000000000000 ) ) ;
#4592 = AXIS2_PLACEMENT_3D ( 'NONE', #6820, #4246, #3365 ) ;
#4593 = ORIENTED_EDGE ( 'NONE', *, *, #5320, .F. ) ;
#4594 = EDGE_CURVE ( 'NONE', #1702, #302, #600, .T. ) ;
#4595 = CARTESIAN_POINT ( 'NONE',  ( -61.56765823437498852, 10.59895833299193413, 2.248837904296538515 ) ) ;
#4596 = LINE ( 'NONE', #8000, #856 ) ;
#4597 = CIRCLE ( 'NONE', #10645, 0.5999999999999999778 ) ;
#4598 = CARTESIAN_POINT ( 'NONE',  ( -62.86468353124999453, 14.51562499965860020, 1.500000000000002220 ) ) ;
#4599 = FACE_OUTER_BOUND ( 'NONE', #4247, .T. ) ;
#4600 = ORIENTED_EDGE ( 'NONE', *, *, #5877, .T. ) ;
#4601 = LINE ( 'NONE', #326, #4424 ) ;
#4602 = VERTEX_POINT ( 'NONE', #5746 ) ;
#4603 = DIRECTION ( 'NONE',  ( -0.000000000000000000, -1.000000000000000000, -0.000000000000000000 ) ) ;
#4604 = CARTESIAN_POINT ( 'NONE',  ( -61.49999999999998579, 8.041666666666667851, 0.6339745962155628467 ) ) ;
#4605 = VECTOR ( 'NONE', #10887, 1000.000000000000000 ) ;
#4606 = DIRECTION ( 'NONE',  ( -0.000000000000000000, -0.000000000000000000, -1.000000000000000000 ) ) ;
#4607 = LINE ( 'NONE', #9610, #7435 ) ;
#4608 = CARTESIAN_POINT ( 'NONE',  ( 150.0000000000000284, 2.500000000000000000, 4.000000000000000000 ) ) ;
#4609 = CARTESIAN_POINT ( 'NONE',  ( -62.43234176562499016, 14.80729166632526805, 2.248837904296538071 ) ) ;
#4610 = CARTESIAN_POINT ( 'NONE',  ( -62.86468353124998032, 9.932291666325269830, 1.000774730468978246 ) ) ;
#4611 = UNCERTAINTY_MEASURE_WITH_UNIT (LENGTH_MEASURE( 1.000000000000000082E-05 ), #2122, 'distance_accuracy_value', 'NONE');
#4612 =( GEOMETRIC_REPRESENTATION_CONTEXT ( 3 ) GLOBAL_UNCERTAINTY_ASSIGNED_CONTEXT ( ( #9944 ) ) GLOBAL_UNIT_ASSIGNED_CONTEXT ( ( #9927, #7481, #9144 ) ) REPRESENTATION_CONTEXT ( 'NONE', 'WORKASPACE' ) );
#4613 =( NAMED_UNIT ( * ) SI_UNIT ( $, .STERADIAN. ) SOLID_ANGLE_UNIT ( ) );
#4614 = DIRECTION ( 'NONE',  ( 0.000000000000000000, 0.000000000000000000, -1.000000000000000000 ) ) ;
#4615 = ADVANCED_FACE ( 'NONE', ( #5852 ), #5063, .T. ) ;
#4616 = CARTESIAN_POINT ( 'NONE',  ( -61.99999999999998579, 11.07812499965860020, 2.498450539062049724 ) ) ;
#4617 = DIRECTION ( 'NONE',  ( -0.000000000000000000, -0.000000000000000000, -1.000000000000000000 ) ) ;
#4618 = VERTEX_POINT ( 'NONE', #3297 ) ;
#4619 = CARTESIAN_POINT ( 'NONE',  ( -62.26794919243111082, 14.32366454968462932, 0.5000000000000013323 ) ) ;
#4620 = PRODUCT_DEFINITION_CONTEXT ( 'detailed design', #1873, 'design' ) ;
#4621 = DIRECTION ( 'NONE',  ( 0.000000000000000000, 0.000000000000000000, -1.000000000000000000 ) ) ;
#4622 = ORIENTED_EDGE ( 'NONE', *, *, #10648, .F. ) ;
#4623 = CARTESIAN_POINT ( 'NONE',  ( -61.99999999999998579, 10.28124999931720218, 0.5000000000000013323 ) ) ;
#4624 = CARTESIAN_POINT ( 'NONE',  ( -62.43234176562498305, 13.16145833299193413, 0.7511620957034662593 ) ) ;
#4625 = CARTESIAN_POINT ( 'NONE',  ( -62.43234176562499016, 10.24479166632526805, 2.248837904296538071 ) ) ;
#4626 = VERTEX_POINT ( 'NONE', #8461 ) ;
#4627 = CARTESIAN_POINT ( 'NONE',  ( -62.86468353124998032, 11.49479166632526805, 1.000774730468978024 ) ) ;
#4628 = DIRECTION ( 'NONE',  ( 0.000000000000000000, 0.000000000000000000, 1.000000000000000000 ) ) ;
#4629 = CARTESIAN_POINT ( 'NONE',  ( -61.99999999999998579, 15.01562499965860198, 2.498450539062049724 ) ) ;
#4630 = CARTESIAN_POINT ( 'NONE',  ( -60.99999999999998579, 14.44791666598387003, 2.077350269189628840 ) ) ;
#4631 = CARTESIAN_POINT ( 'NONE',  ( -60.99999999999998579, 14.69791666598386826, 2.077350269189628840 ) ) ;
#4632 = ORIENTED_EDGE ( 'NONE', *, *, #2292, .F. ) ;
#4633 = EDGE_CURVE ( 'NONE', #5222, #3446, #6539, .T. ) ;
#4634 = CYLINDRICAL_SURFACE ( 'NONE', #1649, 0.9999999999999981126 ) ;
#4635 = ORIENTED_EDGE ( 'NONE', *, *, #3970, .T. ) ;
#4636 =( BOUNDED_CURVE ( )  B_SPLINE_CURVE ( 2, ( #9321, #4310, #7827, #823, #98 ),
 .UNSPECIFIED., .F., .T. ) 
 B_SPLINE_CURVE_WITH_KNOTS ( ( 3, 2, 3 ),
 ( 0.000000000000000000, 0.005208333333333333044, 0.007812499999999973112 ),
 .UNSPECIFIED. ) 
 CURVE ( )  GEOMETRIC_REPRESENTATION_ITEM ( )  RATIONAL_B_SPLINE_CURVE ( ( 1.000000000000000000, 0.8660254037844387076, 1.000000000000000000, 0.9330127018922200755, 0.9330127018922194093 ) ) 
 REPRESENTATION_ITEM ( '' )  );
#4637 = CARTESIAN_POINT ( 'NONE',  ( -61.56765823437498142, 12.86979166632526805, 0.7511620957034663704 ) ) ;
#4638 = CARTESIAN_POINT ( 'NONE',  ( -61.13531646874998415, 9.098958332991934128, 1.000774730468978468 ) ) ;
#4639 = DIRECTION ( 'NONE',  ( -0.000000000000000000, -1.000000000000000000, -0.000000000000000000 ) ) ;
#4640 = ORIENTED_EDGE ( 'NONE', *, *, #7550, .F. ) ;
#4641 = CARTESIAN_POINT ( 'NONE',  ( -60.99999999999998579, 13.02083333333333215, 0.9226497308103762673 ) ) ;
#4642 = FACE_OUTER_BOUND ( 'NONE', #8084, .T. ) ;
#4643 = CARTESIAN_POINT ( 'NONE',  ( -61.13531646874998415, 14.14062499965860198, 1.500000000000002220 ) ) ;
#4644 = CARTESIAN_POINT ( 'NONE',  ( -62.49999999999998579, 14.30208333265053611, 0.6339745962155627357 ) ) ;
#4645 = CARTESIAN_POINT ( 'NONE',  ( -61.49999999999998579, 10.67708333265053611, 2.366025403784441927 ) ) ;
#4646 = ORIENTED_EDGE ( 'NONE', *, *, #2587, .T. ) ;
#4647 = CARTESIAN_POINT ( 'NONE',  ( -62.99999999999998579, 14.85416666666666607, 0.9226497308103756012 ) ) ;
#4648 = CARTESIAN_POINT ( 'NONE',  ( -62.86468353124998742, 12.97395833299193413, 1.999225269531025972 ) ) ;
#4649 = LINE ( 'NONE', #9879, #130 ) ;
#4650 = EDGE_LOOP ( 'NONE', ( #8170, #10143, #6825, #7130 ) ) ;
#4651 = AXIS2_PLACEMENT_3D ( 'NONE', #1451, #4986, #3321 ) ;
#4652 = CARTESIAN_POINT ( 'NONE',  ( -61.56765823437498852, 10.09895833299193413, 2.248837904296538515 ) ) ;
#4653 = LINE ( 'NONE', #8060, #3885 ) ;
#4654 = DIRECTION ( 'NONE',  ( 0.000000000000000000, -1.000000000000000000, 0.000000000000000000 ) ) ;
#4655 = CARTESIAN_POINT ( 'NONE',  ( -60.99999999999998579, 8.947916665983868256, 2.077350269189628840 ) ) ;
#4656 = ORIENTED_EDGE ( 'NONE', *, *, #2466, .T. ) ;
#4657 = DIRECTION ( 'NONE',  ( -0.000000000000000000, -1.000000000000000000, -0.000000000000000000 ) ) ;
#4658 = EDGE_CURVE ( 'NONE', #3634, #7235, #2518, .T. ) ;
#4659 = ORIENTED_EDGE ( 'NONE', *, *, #4239, .F. ) ;
#4660 = CARTESIAN_POINT ( 'NONE',  ( -62.26794919243111082, 15.14508544963257108, 2.500000000000003109 ) ) ;
#4661 = CARTESIAN_POINT ( 'NONE',  ( -62.99999999999998579, 10.12500000000000000, 1.500000000000001998 ) ) ;
#4662 = CARTESIAN_POINT ( 'NONE',  ( -61.99999999999998579, 11.18750000000000000, 2.500000000000002665 ) ) ;
#4663 = DIRECTION ( 'NONE',  ( -0.000000000000000000, -0.000000000000000000, -1.000000000000000000 ) ) ;
#4664 =( BOUNDED_CURVE ( )  B_SPLINE_CURVE ( 2, ( #9358, #8476, #10083, #3470, #4295, #5027, #6660, #10239, #709 ),
 .UNSPECIFIED., .F., .F. ) 
 B_SPLINE_CURVE_WITH_KNOTS ( ( 3, 2, 2, 2, 3 ),
 ( 0.3984375000000000000, 0.4010416666666666852, 0.4062500000000000000, 0.4114583333333333148, 0.4140625000000000000 ),
 .UNSPECIFIED. ) 
 CURVE ( )  GEOMETRIC_REPRESENTATION_ITEM ( )  RATIONAL_B_SPLINE_CURVE ( ( 0.9330127018922194093, 0.9330127018922194093, 1.000000000000000000, 0.8660254037844387076, 1.000000000000000000, 0.8660254037844387076, 1.000000000000000000, 0.9330127018922194093, 0.9330127018922194093 ) ) 
 REPRESENTATION_ITEM ( '' )  );
#4665 = DIRECTION ( 'NONE',  ( -0.000000000000000000, 1.000000000000000000, 0.000000000000000000 ) ) ;
#4666 = VECTOR ( 'NONE', #6917, 1000.000000000000000 ) ;
#4667 = CARTESIAN_POINT ( 'NONE',  ( -62.86468353124998742, 10.22395833299193413, 1.999225269531025972 ) ) ;
#4668 = CARTESIAN_POINT ( 'NONE',  ( 145.0000000000000284, 5.500000000000000000, 3.000000000000000888 ) ) ;
#4669 = CARTESIAN_POINT ( 'NONE',  ( -61.56765823437498142, 10.68229166632526805, 0.7511620957034663704 ) ) ;
#4670 = CARTESIAN_POINT ( 'NONE',  ( -103.9999999999999858, 0.000000000000000000, 10.99999999999999289 ) ) ;
#4671 = ORIENTED_EDGE ( 'NONE', *, *, #8511, .T. ) ;
#4672 = DIRECTION ( 'NONE',  ( 0.000000000000000000, 1.000000000000000000, 0.000000000000000000 ) ) ;
#4673 = CARTESIAN_POINT ( 'NONE',  ( -62.49999999999998579, 9.166666666666666075, 2.366025403784441483 ) ) ;
#4674 = VECTOR ( 'NONE', #10556, 1000.000000000000000 ) ;
#4675 = ORIENTED_EDGE ( 'NONE', *, *, #10296, .T. ) ;
#4676 = CARTESIAN_POINT ( 'NONE',  ( -60.99999999999998579, 10.23958333265053788, 0.9226497308103762673 ) ) ;
#4677 = EDGE_CURVE ( 'NONE', #3276, #8026, #3053, .T. ) ;
#4678 = CARTESIAN_POINT ( 'NONE',  ( -62.86468353124998742, 12.97395833299193413, 1.999225269531025972 ) ) ;
#4679 = CARTESIAN_POINT ( 'NONE',  ( -61.56765823437498852, 10.28645833299193413, 2.248837904296538515 ) ) ;
#4680 =( LENGTH_UNIT ( ) NAMED_UNIT ( * ) SI_UNIT ( .MILLI., .METRE. ) );
#4681 = ORIENTED_EDGE ( 'NONE', *, *, #445, .T. ) ;
#4682 = CARTESIAN_POINT ( 'NONE',  ( -60.99999999999998579, 8.447916665983870033, 2.077350269189628840 ) ) ;
#4683 = CARTESIAN_POINT ( 'NONE',  ( -62.43234176562499016, 11.55729166632526805, 2.248837904296538071 ) ) ;
#4684 = PRODUCT_CONTEXT ( 'NONE', #233, 'mechanical' ) ;
#4685 = CARTESIAN_POINT ( 'NONE',  ( -62.43234176562498305, 15.41145833299193590, 0.7511620957034662593 ) ) ;
#4686 = CARTESIAN_POINT ( 'NONE',  ( -62.99999999999998579, 14.86458333265053611, 2.077350269189627952 ) ) ;
#4687 = CARTESIAN_POINT ( 'NONE',  ( 150.0000000000000284, -8.000000000000000000, 0.000000000000000000 ) ) ;
#4688 = ORIENTED_EDGE ( 'NONE', *, *, #7597, .F. ) ;
#4689 = VERTEX_POINT ( 'NONE', #1688 ) ;
#4690 = ADVANCED_BREP_SHAPE_REPRESENTATION ( '', ( #4847, #2307 ), #351 ) ;
#4691 = CARTESIAN_POINT ( 'NONE',  ( -61.56765823437498142, 13.36979166632526805, 0.7511620957034663704 ) ) ;
#4692 = CARTESIAN_POINT ( 'NONE',  ( -62.43234176562498305, 8.161458332991934128, 0.7511620957034662593 ) ) ;
#4693 = CARTESIAN_POINT ( 'NONE',  ( -61.49999999999998579, 11.70833333333333215, 2.366025403784441927 ) ) ;
#4694 = ORIENTED_EDGE ( 'NONE', *, *, #7985, .F. ) ;
#4695 = CARTESIAN_POINT ( 'NONE',  ( -61.49999999999998579, 12.04166666666666607, 0.6339745962155628467 ) ) ;
#4696 = CARTESIAN_POINT ( 'NONE',  ( -62.99999999999998579, 11.11458333265053611, 2.077350269189627952 ) ) ;
#4697 = PRESENTATION_STYLE_ASSIGNMENT (( #1327 ) ) ;
#4698 = LINE ( 'NONE', #2447, #3005 ) ;
#4699 = CARTESIAN_POINT ( 'NONE',  ( -62.49999999999998579, 10.13541666598387003, 2.366025403784441483 ) ) ;
#4700 = VERTEX_POINT ( 'NONE', #1477 ) ;
#4701 = EDGE_CURVE ( 'NONE', #4192, #8205, #4854, .T. ) ;
#4702 = CARTESIAN_POINT ( 'NONE',  ( 150.0000000000000000, -2.500000000000000444, 3.000000000000000000 ) ) ;
#4703 = CARTESIAN_POINT ( 'NONE',  ( -61.13531646874998415, 12.05729166632526628, 1.999225269531026417 ) ) ;
#4704 = ORIENTED_EDGE ( 'NONE', *, *, #9696, .F. ) ;
#4705 = CARTESIAN_POINT ( 'NONE',  ( -62.86468353124998032, 11.49479166632526805, 1.000774730468978246 ) ) ;
#4706 = CARTESIAN_POINT ( 'NONE',  ( -61.49999999999998579, 12.17708333265053611, 2.366025403784441927 ) ) ;
#4707 = EDGE_CURVE ( 'NONE', #3104, #1612, #1963, .T. ) ;
#4708 = CARTESIAN_POINT ( 'NONE',  ( -61.13531646874998415, 15.36979166632526983, 1.999225269531026417 ) ) ;
#4709 = DIRECTION ( 'NONE',  ( -0.000000000000000000, -1.000000000000000000, -0.000000000000000000 ) ) ;
#4710 = EDGE_LOOP ( 'NONE', ( #10272, #7654, #7633 ) ) ;
#4711 = DIRECTION ( 'NONE',  ( -0.000000000000000000, -1.000000000000000000, -0.000000000000000000 ) ) ;
#4712 = ORIENTED_EDGE ( 'NONE', *, *, #2266, .F. ) ;
#4713 = CARTESIAN_POINT ( 'NONE',  ( -60.99999999999998579, 9.479166666666666075, 2.077350269189628840 ) ) ;
#4714 = FACE_OUTER_BOUND ( 'NONE', #115, .T. ) ;
#4715 = CARTESIAN_POINT ( 'NONE',  ( -60.99999999999998579, 11.97916666666666785, 2.077350269189628840 ) ) ;
#4716 = FACE_OUTER_BOUND ( 'NONE', #9096, .T. ) ;
#4717 = CARTESIAN_POINT ( 'NONE',  ( -61.13531646874998415, 10.57812499965860198, 1.500000000000002220 ) ) ;
#4718 = CARTESIAN_POINT ( 'NONE',  ( -60.99999999999998579, 8.218749999317202182, 1.500000000000002220 ) ) ;
#4719 = CARTESIAN_POINT ( 'NONE',  ( -61.99999999999998579, 12.32812499965860376, 2.498450539062049724 ) ) ;
#4720 = DIRECTION ( 'NONE',  ( 0.000000000000000000, 0.000000000000000000, 1.000000000000000000 ) ) ;
#4721 = ORIENTED_EDGE ( 'NONE', *, *, #9877, .T. ) ;
#4722 = CARTESIAN_POINT ( 'NONE',  ( -62.99999999999998579, 15.39583333333333393, 2.077350269189627952 ) ) ;
#4723 = ORIENTED_EDGE ( 'NONE', *, *, #3087, .T. ) ;
#4724 = CARTESIAN_POINT ( 'NONE',  ( -62.49999999999998579, 10.13541666598387003, 2.366025403784441483 ) ) ;
#4725 = EDGE_CURVE ( 'NONE', #4541, #5466, #3361, .T. ) ;
#4726 = CARTESIAN_POINT ( 'NONE',  ( -62.86468353124999453, 14.20312499965860020, 1.500000000000002220 ) ) ;
#4727 = CARTESIAN_POINT ( 'NONE',  ( -62.43234176562499016, 10.74479166632526805, 2.248837904296538071 ) ) ;
#4728 = DIRECTION ( 'NONE',  ( -0.000000000000000000, -0.000000000000000000, -1.000000000000000000 ) ) ;
#4729 = ORIENTED_EDGE ( 'NONE', *, *, #1550, .T. ) ;
#4730 = LINE ( 'NONE', #528, #1563 ) ;
#4731 = CARTESIAN_POINT ( 'NONE',  ( -61.13531646874998415, 10.89062499965860020, 1.500000000000002220 ) ) ;
#4732 = EDGE_CURVE ( 'NONE', #8685, #3802, #7799, .T. ) ;
#4733 =( LENGTH_UNIT ( ) NAMED_UNIT ( * ) SI_UNIT ( .MILLI., .METRE. ) );
#4734 = DIRECTION ( 'NONE',  ( -0.000000000000000000, -1.000000000000000000, -0.000000000000000000 ) ) ;
#4735 = CARTESIAN_POINT ( 'NONE',  ( -61.99999999999998579, 8.328124999658601979, 2.498450539062049724 ) ) ;
#4736 = PLANE ( 'NONE',  #1314 ) ;
#4737 = ORIENTED_EDGE ( 'NONE', *, *, #10261, .T. ) ;
#4738 = ADVANCED_FACE ( 'NONE', ( #1794 ), #5331, .F. ) ;
#4739 = CARTESIAN_POINT ( 'NONE',  ( -61.38196601871477043, 16.00549858343031673, 0.7021215470841072337 ) ) ;
#4740 = VERTEX_POINT ( 'NONE', #1852 ) ;
#4741 = PRODUCT_RELATED_PRODUCT_CATEGORY ( 'part', '', ( #7593 ) ) ;
#4742 = CARTESIAN_POINT ( 'NONE',  ( -62.43234176562499016, 13.49479166632526805, 2.248837904296538071 ) ) ;
#4743 = CARTESIAN_POINT ( 'NONE',  ( -61.56765823437498142, 9.619791666325268054, 0.7511620957034663704 ) ) ;
#4744 = VECTOR ( 'NONE', #10038, 1000.000000000000000 ) ;
#4745 = FACE_OUTER_BOUND ( 'NONE', #877, .T. ) ;
#4746 = ORIENTED_EDGE ( 'NONE', *, *, #2661, .T. ) ;
#4747 = CARTESIAN_POINT ( 'NONE',  ( -61.99999999999998579, 13.06250000000000355, 0.3452994616207497591 ) ) ;
#4748 = CARTESIAN_POINT ( 'NONE',  ( -57.99999999999998579, -14.00000000000001243, 3.000000000000000000 ) ) ;
#4749 = FILL_AREA_STYLE_COLOUR ( '', #3534 ) ;
#4750 = CARTESIAN_POINT ( 'NONE',  ( -62.99999999999998579, 11.09374999931720218, 1.500000000000001998 ) ) ;
#4751 = ADVANCED_FACE ( 'NONE', ( #2794 ), #6182, .T. ) ;
#4752 = VECTOR ( 'NONE', #10055, 1000.000000000000000 ) ;
#4753 = CARTESIAN_POINT ( 'NONE',  ( 0.2307700686259116507, -0.2500000000000000555, 1.812750528907548730 ) ) ;
#4754 = CARTESIAN_POINT ( 'NONE',  ( -61.99999999999998579, 12.01562499965860020, 2.498450539062049724 ) ) ;
#4755 = LINE ( 'NONE', #553, #6700 ) ;
#4756 = ORIENTED_EDGE ( 'NONE', *, *, #5697, .F. ) ;
#4757 = VECTOR ( 'NONE', #8025, 1000.000000000000000 ) ;
#4758 = CARTESIAN_POINT ( 'NONE',  ( -61.13531646874998415, 11.61979166632526983, 1.999225269531026417 ) ) ;
#4759 = CARTESIAN_POINT ( 'NONE',  ( -61.99999999999998579, 12.53124999931720396, 0.5000000000000013323 ) ) ;
#4760 = VECTOR ( 'NONE', #1490, 1000.000000000000000 ) ;
#4761 = CARTESIAN_POINT ( 'NONE',  ( -61.99999999999998579, 8.687500000000000000, 2.500000000000002665 ) ) ;
#4762 = VERTEX_POINT ( 'NONE', #182 ) ;
#4763 = EDGE_CURVE ( 'NONE', #9934, #1925, #7848, .T. ) ;
#4764 = CARTESIAN_POINT ( 'NONE',  ( -61.99999999999998579, 26.00000000000000355, -1.000000000000000000 ) ) ;
#4765 = AXIS2_PLACEMENT_3D ( 'NONE', #10730, #10774, #2123 ) ;
#4766 = AXIS2_PLACEMENT_3D ( 'NONE', #7840, #7731, #10268 ) ;
#4767 = ORIENTED_EDGE ( 'NONE', *, *, #960, .F. ) ;
#4768 = DIRECTION ( 'NONE',  ( 0.000000000000000000, 0.000000000000000000, -1.000000000000000000 ) ) ;
#4769 = ADVANCED_FACE ( 'NONE', ( #6123 ), #9345, .F. ) ;
#4770 = CARTESIAN_POINT ( 'NONE',  ( -62.99999999999998579, 9.854166666666666075, 0.9226497308103756012 ) ) ;
#4771 = DIRECTION ( 'NONE',  ( -0.8571673013836855759, 0.000000000000000000, -0.5150380737757257466 ) ) ;
#4772 = CARTESIAN_POINT ( 'NONE',  ( -61.99999999999998579, 16.00000000000000000, 1.500000000000002220 ) ) ;
#4773 = MANIFOLD_SOLID_BREP ( 'Slot', #7842 ) ;
#4774 = CARTESIAN_POINT ( 'NONE',  ( -62.99999999999998579, 14.86458333265053611, 2.077350269189627952 ) ) ;
#4775 = CIRCLE ( 'NONE', #9761, 1.099999999999989875 ) ;
#4776 = CARTESIAN_POINT ( 'NONE',  ( -62.49999999999998579, 8.552083332650536107, 0.6339745962155627357 ) ) ;
#4777 = CARTESIAN_POINT ( 'NONE',  ( -61.99999999999998579, 11.45312499965860020, 0.5015494609379544944 ) ) ;
#4778 = CARTESIAN_POINT ( 'NONE',  ( -62.26794919243111082, 9.145085449632572860, 2.500000000000004885 ) ) ;
#4779 = ORIENTED_EDGE ( 'NONE', *, *, #4001, .F. ) ;
#4780 = DIRECTION ( 'NONE',  ( -1.000000000000000000, -0.000000000000000000, -0.000000000000000000 ) ) ;
#4781 = CARTESIAN_POINT ( 'NONE',  ( -61.99999999999998579, 15.18750000000000000, 2.500000000000002665 ) ) ;
#4782 = VECTOR ( 'NONE', #1506, 1000.000000000000000 ) ;
#4783 = VERTEX_POINT ( 'NONE', #6069 ) ;
#4784 = CARTESIAN_POINT ( 'NONE',  ( -61.49999999999998579, 14.17708333265053611, 2.366025403784441927 ) ) ;
#4785 = CARTESIAN_POINT ( 'NONE',  ( -61.99999999999998579, 14.39062499965859843, 0.5015494609379544944 ) ) ;
#4786 = CARTESIAN_POINT ( 'NONE',  ( -61.13531646874998415, 10.57812499965860198, 1.500000000000002220 ) ) ;
#4787 = CARTESIAN_POINT ( 'NONE',  ( -60.99999999999998579, 11.69791666598387181, 2.077350269189628840 ) ) ;
#4788 = ORIENTED_EDGE ( 'NONE', *, *, #10096, .T. ) ;
#4789 = CARTESIAN_POINT ( 'NONE',  ( -61.99999999999998579, 16.00000000000000000, 2.500000000000000444 ) ) ;
#4790 = CARTESIAN_POINT ( 'NONE',  ( -61.13531646874997705, 10.86979166632526805, 1.999225269531026417 ) ) ;
#4791 = CARTESIAN_POINT ( 'NONE',  ( -62.99999999999998579, 13.57291666598387359, 0.9226497308103756012 ) ) ;
#4792 = VECTOR ( 'NONE', #4146, 1000.000000000000000 ) ;
#4793 = CARTESIAN_POINT ( 'NONE',  ( -62.49999999999998579, 15.88541666598386826, 2.366025403784441483 ) ) ;
#4794 = DIRECTION ( 'NONE',  ( -1.000000000000000000, 0.000000000000000000, 0.000000000000000000 ) ) ;
#4795 = ORIENTED_EDGE ( 'NONE', *, *, #1929, .F. ) ;
#4796 = ADVANCED_FACE ( 'NONE', ( #3453 ), #1304, .F. ) ;
#4797 = LINE ( 'NONE', #4017, #7987 ) ;
#4798 = LINE ( 'NONE', #3810, #4477 ) ;
#4799 =( BOUNDED_CURVE ( )  B_SPLINE_CURVE ( 2, ( #10792, #8294, #584, #4791, #8251, #4013, #3859, #2396, #4893 ),
 .UNSPECIFIED., .F., .T. ) 
 B_SPLINE_CURVE_WITH_KNOTS ( ( 3, 2, 2, 2, 3 ),
 ( 0.6640625000000000000, 0.6666666666666666297, 0.6718750000000000000, 0.6770833333333333703, 0.6796875000000000000 ),
 .UNSPECIFIED. ) 
 CURVE ( )  GEOMETRIC_REPRESENTATION_ITEM ( )  RATIONAL_B_SPLINE_CURVE ( ( 0.9330127018922194093, 0.9330127018922194093, 1.000000000000000000, 0.8660254037844387076, 1.000000000000000000, 0.8660254037844387076, 1.000000000000000000, 0.9330127018922194093, 0.9330127018922194093 ) ) 
 REPRESENTATION_ITEM ( '' )  );
#4800 = EDGE_CURVE ( 'NONE', #947, #2754, #5704, .T. ) ;
#4801 = CARTESIAN_POINT ( 'NONE',  ( -62.43234176562498305, 13.66145833299193413, 0.7511620957034662593 ) ) ;
#4802 = CARTESIAN_POINT ( 'NONE',  ( -61.13531646874998415, 10.32812499965860198, 1.500000000000002220 ) ) ;
#4803 = CARTESIAN_POINT ( 'NONE',  ( -62.26794919243111082, 10.54241454900183506, 0.4999999999999982792 ) ) ;
#4804 = EDGE_LOOP ( 'NONE', ( #438, #8620, #6062, #3337 ) ) ;
#4805 = CARTESIAN_POINT ( 'NONE',  ( -62.99999999999998579, 13.85416666666666785, 0.9226497308103756012 ) ) ;
#4806 = CARTESIAN_POINT ( 'NONE',  ( -105.0000000000000000, -2.500000000000000000, 4.000000000000000000 ) ) ;
#4807 = CARTESIAN_POINT ( 'NONE',  ( -62.99999999999998579, 11.84374999931720218, 1.500000000000001998 ) ) ;
#4808 = PLANE ( 'NONE',  #2428 ) ;
#4809 = CARTESIAN_POINT ( 'NONE',  ( -61.56765823437498142, 12.61979166632526805, 0.7511620957034663704 ) ) ;
#4810 = DIRECTION ( 'NONE',  ( 0.000000000000000000, 0.000000000000000000, -1.000000000000000000 ) ) ;
#4811 = ORIENTED_EDGE ( 'NONE', *, *, #3757, .F. ) ;
#4812 = EDGE_CURVE ( 'NONE', #3446, #607, #1183, .T. ) ;
#4813 = CARTESIAN_POINT ( 'NONE',  ( -62.86468353124998742, 12.03645833299193413, 1.999225269531025972 ) ) ;
#4814 = PLANE ( 'NONE',  #1927 ) ;
#4815 = VECTOR ( 'NONE', #2091, 1000.000000000000000 ) ;
#4816 = CARTESIAN_POINT ( 'NONE',  ( -61.13531646874998415, 15.64062499965860198, 1.500000000000002220 ) ) ;
#4817 = ORIENTED_EDGE ( 'NONE', *, *, #6168, .T. ) ;
#4818 = PLANE ( 'NONE',  #8701 ) ;
#4819 = EDGE_LOOP ( 'NONE', ( #134, #99 ) ) ;
#4820 = CARTESIAN_POINT ( 'NONE',  ( -62.99999999999998579, 9.843749999317202182, 1.500000000000001998 ) ) ;
#4821 = CARTESIAN_POINT ( 'NONE',  ( -62.49999999999998579, 9.666666666666667851, 2.366025403784441483 ) ) ;
#4822 = DIRECTION ( 'NONE',  ( -0.000000000000000000, -1.000000000000000000, -0.000000000000000000 ) ) ;
#4823 = CARTESIAN_POINT ( 'NONE',  ( -61.13531646874998415, 8.140624999658601979, 1.500000000000002220 ) ) ;
#4824 = CARTESIAN_POINT ( 'NONE',  ( -62.26794919243111082, 14.89508544963257286, 2.500000000000003109 ) ) ;
#4825 = DIRECTION ( 'NONE',  ( -0.000000000000000000, -0.000000000000000000, 1.000000000000000000 ) ) ;
#4826 = VECTOR ( 'NONE', #2833, 1000.000000000000000 ) ;
#4827 = CIRCLE ( 'NONE', #7500, 1.099999999999989875 ) ;
#4828 = CARTESIAN_POINT ( 'NONE',  ( -61.13531646874998415, 11.66145833299193590, 1.000774730468978468 ) ) ;
#4829 = CARTESIAN_POINT ( 'NONE',  ( -62.99999999999998579, 10.64583333333333570, 2.077350269189627952 ) ) ;
#4830 = EDGE_LOOP ( 'NONE', ( #376, #10531, #10716, #5166 ) ) ;
#4831 = CARTESIAN_POINT ( 'NONE',  ( -61.99999999999998579, 15.31250000000000000, 0.5000000000000013323 ) ) ;
#4832 = EDGE_CURVE ( 'NONE', #4783, #1148, #6994, .T. ) ;
#4833 = CYLINDRICAL_SURFACE ( 'NONE', #9451, 0.9999999999999981126 ) ;
#4834 = ORIENTED_EDGE ( 'NONE', *, *, #2487, .T. ) ;
#4835 = COLOUR_RGB ( '',0.8941176470588234615, 0.8941176470588234615, 0.8941176470588234615 ) ;
#4836 = CARTESIAN_POINT ( 'NONE',  ( -61.99999999999998579, 13.31249999999999822, 0.5000000000000013323 ) ) ;
#4837 = CARTESIAN_POINT ( 'NONE',  ( -62.86468353124998742, 13.22395833299193235, 1.999225269531025972 ) ) ;
#4838 = CARTESIAN_POINT ( 'NONE',  ( -61.56765823437498852, 10.53645833299193413, 2.248837904296538515 ) ) ;
#4839 = CARTESIAN_POINT ( 'NONE',  ( -62.99999999999998579, 8.322916665983870033, 0.9226497308103756012 ) ) ;
#4840 = CARTESIAN_POINT ( 'NONE',  ( -61.99999999999999289, 11.95312499965860198, 0.5015494609379544944 ) ) ;
#4841 = CARTESIAN_POINT ( 'NONE',  ( -61.13531646874998415, 15.36979166632526983, 1.999225269531026417 ) ) ;
#4842 = ITEM_DEFINED_TRANSFORMATION ( 'NONE', 'NONE', #2478,  #2307 ) ;
#4843 = CARTESIAN_POINT ( 'NONE',  ( -61.99999999999998579, 26.00000000000000355, 1.500000000000002220 ) ) ;
#4844 = CARTESIAN_POINT ( 'NONE',  ( -60.99999999999998579, 16.21874999931720396, 1.500000000000002220 ) ) ;
#4845 = LINE ( 'NONE', #5002, #1802 ) ;
#4846 = VERTEX_POINT ( 'NONE', #3854 ) ;
#4847 = MANIFOLD_SOLID_BREP ( 'Cut-Extrude1', #10505 ) ;
#4848 = DIRECTION ( 'NONE',  ( -1.000000000000000000, -0.000000000000000000, -0.000000000000000000 ) ) ;
#4849 = EDGE_CURVE ( 'NONE', #1608, #5268, #10686, .T. ) ;
#4850 = LINE ( 'NONE', #8257, #5546 ) ;
#4851 = CARTESIAN_POINT ( 'NONE',  ( -62.86468353124999453, 14.47395833299193413, 1.999225269531025750 ) ) ;
#4852 = CARTESIAN_POINT ( 'NONE',  ( -62.86468353124998742, 9.723958332991934128, 1.999225269531025972 ) ) ;
#4853 = APPLICATION_CONTEXT ( 'automotive_design' ) ;
#4854 = LINE ( 'NONE', #4023, #2008 ) ;
#4855 = ORIENTED_EDGE ( 'NONE', *, *, #1807, .T. ) ;
#4856 = CARTESIAN_POINT ( 'NONE',  ( -62.99999999999998579, 14.35416666666666785, 0.9226497308103756012 ) ) ;
#4857 = CIRCLE ( 'NONE', #10720, 1.099999999999989875 ) ;
#4858 = CARTESIAN_POINT ( 'NONE',  ( -61.99999999999998579, 13.28124999931720041, 0.5000000000000013323 ) ) ;
#4859 =( NAMED_UNIT ( * ) SI_UNIT ( $, .STERADIAN. ) SOLID_ANGLE_UNIT ( ) );
#4860 = CARTESIAN_POINT ( 'NONE',  ( -60.99999999999998579, 11.44791666598387003, 2.077350269189628840 ) ) ;
#4861 = EDGE_CURVE ( 'NONE', #6076, #5356, #7074, .T. ) ;
#4862 =( BOUNDED_CURVE ( )  B_SPLINE_CURVE ( 2, ( #1464, #8194, #10787, #4839, #9175, #1561, #4944, #8247, #9907 ),
 .UNSPECIFIED., .F., .F. ) 
 B_SPLINE_CURVE_WITH_KNOTS ( ( 3, 2, 2, 2, 3 ),
 ( 0.007812499999999973112, 0.01041666666666666609, 0.01562500000000000000, 0.02083333333333333218, 0.02343749999999996531 ),
 .UNSPECIFIED. ) 
 CURVE ( )  GEOMETRIC_REPRESENTATION_ITEM ( )  RATIONAL_B_SPLINE_CURVE ( ( 0.9330127018922194093, 0.9330127018922187432, 1.000000000000000000, 0.8660254037844387076, 1.000000000000000000, 0.8660254037844387076, 1.000000000000000000, 0.9330127018922202975, 0.9330127018922194093 ) ) 
 REPRESENTATION_ITEM ( '' )  );
#4863 = CARTESIAN_POINT ( 'NONE',  ( -62.86468353124998032, 13.93229166632526805, 1.000774730468978246 ) ) ;
#4864 = ORIENTED_EDGE ( 'NONE', *, *, #9058, .T. ) ;
#4865 = CARTESIAN_POINT ( 'NONE',  ( -62.86468353124998742, 11.28645833299193590, 1.999225269531025972 ) ) ;
#4866 = DIRECTION ( 'NONE',  ( -0.000000000000000000, -0.000000000000000000, -1.000000000000000000 ) ) ;
#4867 = EDGE_CURVE ( 'NONE', #7493, #8372, #3076, .T. ) ;
#4868 = CARTESIAN_POINT ( 'NONE',  ( -62.43234176562499016, 16.05729166632526628, 2.248837904296538071 ) ) ;
#4869 = ORIENTED_EDGE ( 'NONE', *, *, #1610, .F. ) ;
#4870 = CARTESIAN_POINT ( 'NONE',  ( -49.99999999999998579, -15.00000000000001243, 0.000000000000000000 ) ) ;
#4871 = ADVANCED_FACE ( 'NONE', ( #1126 ), #9800, .F. ) ;
#4872 = ORIENTED_EDGE ( 'NONE', *, *, #4701, .F. ) ;
#4873 = DIRECTION ( 'NONE',  ( 1.000000000000000000, 0.000000000000000000, 0.000000000000000000 ) ) ;
#4874 = CARTESIAN_POINT ( 'NONE',  ( -61.99999999999998579, 9.562500000000000000, 0.3452994616207497591 ) ) ;
#4875 = DIRECTION ( 'NONE',  ( -1.000000000000000000, 0.000000000000000000, 0.000000000000000000 ) ) ;
#4876 = CARTESIAN_POINT ( 'NONE',  ( -61.99999999999998579, 8.562500000000000000, 0.5000000000000013323 ) ) ;
#4877 = CARTESIAN_POINT ( 'NONE',  ( -61.73205080756886076, 12.19866454968462932, 2.500000000000003109 ) ) ;
#4878 = DIRECTION ( 'NONE',  ( 0.000000000000000000, 0.000000000000000000, -1.000000000000000000 ) ) ;
#4879 = CARTESIAN_POINT ( 'NONE',  ( -61.13531646874998415, 12.39062499965860198, 1.500000000000002220 ) ) ;
#4880 = CARTESIAN_POINT ( 'NONE',  ( -77.99999999999998579, -11.50000000000000711, 8.000000000000000000 ) ) ;
#4881 = ORIENTED_EDGE ( 'NONE', *, *, #5472, .F. ) ;
#4882 = CARTESIAN_POINT ( 'NONE',  ( -61.99999999999998579, 9.281249999317203958, 0.5000000000000013323 ) ) ;
#4883 = VERTEX_POINT ( 'NONE', #291 ) ;
#4884 = DIRECTION ( 'NONE',  ( -0.000000000000000000, -1.000000000000000000, -0.000000000000000000 ) ) ;
#4885 = CARTESIAN_POINT ( 'NONE',  ( -62.86468353124998742, 13.47395833299193413, 1.999225269531025972 ) ) ;
#4886 = CARTESIAN_POINT ( 'NONE',  ( -62.99999999999998579, 11.85416666666666607, 0.9226497308103756012 ) ) ;
#4887 =( NAMED_UNIT ( * ) SI_UNIT ( $, .STERADIAN. ) SOLID_ANGLE_UNIT ( ) );
#4888 = CARTESIAN_POINT ( 'NONE',  ( -61.99999999999998579, 13.06250000000000178, 0.5000000000000013323 ) ) ;
#4889 = CARTESIAN_POINT ( 'NONE',  ( -61.99999999999999289, 13.07812499965860198, 2.498450539062049724 ) ) ;
#4890 = CARTESIAN_POINT ( 'NONE',  ( -61.13531646874998415, 15.14062499965860020, 1.500000000000002220 ) ) ;
#4891 = DIRECTION ( 'NONE',  ( -0.000000000000000000, -1.000000000000000000, -0.000000000000000000 ) ) ;
#4892 = EDGE_CURVE ( 'NONE', #8034, #9106, #8658, .T. ) ;
#4893 = CARTESIAN_POINT ( 'NONE',  ( -61.99999999999998579, 13.65624999931720218, 2.500000000000002665 ) ) ;
#4894 = CARTESIAN_POINT ( 'NONE',  ( -62.99999999999998579, 15.84374999931720218, 1.500000000000001998 ) ) ;
#4895 = LINE ( 'NONE', #1569, #7147 ) ;
#4896 = EDGE_LOOP ( 'NONE', ( #8275, #9624, #4712, #4971 ) ) ;
#4897 = DIRECTION ( 'NONE',  ( -0.000000000000000000, -0.000000000000000000, 1.000000000000000000 ) ) ;
#4898 = CARTESIAN_POINT ( 'NONE',  ( -105.0000000000000000, -2.500000000000000000, 2.000000000000000000 ) ) ;
#4899 = EDGE_CURVE ( 'NONE', #5865, #6224, #3235, .T. ) ;
#4900 = CARTESIAN_POINT ( 'NONE',  ( -61.56765823437498142, 14.86979166632526805, 0.7511620957034663704 ) ) ;
#4901 = CARTESIAN_POINT ( 'NONE',  ( -61.99999999999998579, 9.390624999658600203, 0.5015494609379544944 ) ) ;
#4902 = CARTESIAN_POINT ( 'NONE',  ( -61.13531646874997705, 16.11979166632526628, 1.999225269531026417 ) ) ;
#4903 = CARTESIAN_POINT ( 'NONE',  ( -60.99999999999998579, 14.48958333265054144, 0.9226497308103762673 ) ) ;
#4904 = ORIENTED_EDGE ( 'NONE', *, *, #2830, .F. ) ;
#4905 = CARTESIAN_POINT ( 'NONE',  ( -61.49999999999998579, 13.54166666666666785, 0.6339745962155628467 ) ) ;
#4906 = EDGE_CURVE ( 'NONE', #10281, #7755, #621, .T. ) ;
#4907 = CARTESIAN_POINT ( 'NONE',  ( -57.99999999999998579, -14.00000000000001243, 3.141811147483251965 ) ) ;
#4908 = CARTESIAN_POINT ( 'NONE',  ( -61.99999999999998579, 11.28124999931720041, 0.3452994616207497591 ) ) ;
#4909 = DIRECTION ( 'NONE',  ( 0.000000000000000000, 0.000000000000000000, -1.000000000000000000 ) ) ;
#4910=STYLED_ITEM('',(#11034),#8606);
#4911 =( REPRESENTATION_RELATIONSHIP ('NONE','NONE', #560, #10405 ) REPRESENTATION_RELATIONSHIP_WITH_TRANSFORMATION ( #7409 )SHAPE_REPRESENTATION_RELATIONSHIP( ) );
#4912 = MANIFOLD_SOLID_BREP ( 'Fillet1', #1629 ) ;
#4913 = CARTESIAN_POINT ( 'NONE',  ( -62.86468353124998742, 13.97395833299193413, 1.999225269531025972 ) ) ;
#4914 = CARTESIAN_POINT ( 'NONE',  ( -61.99999999999997868, 11.43750000000000000, 2.500000000000002665 ) ) ;
#4915 = ORIENTED_EDGE ( 'NONE', *, *, #5750, .F. ) ;
#4916 = CARTESIAN_POINT ( 'NONE',  ( -61.13531646874998415, 11.66145833299193590, 1.000774730468978468 ) ) ;
#4917 =( BOUNDED_CURVE ( )  B_SPLINE_CURVE ( 2, ( #10403, #8524, #9463, #8582, #10180, #2576, #2633, #6969, #7918 ),
 .UNSPECIFIED., .F., .T. ) 
 B_SPLINE_CURVE_WITH_KNOTS ( ( 3, 2, 2, 2, 3 ),
 ( 0.8203125000000000000, 0.8229166666666666297, 0.8281250000000000000, 0.8333333333333333703, 0.8359375000000000000 ),
 .UNSPECIFIED. ) 
 CURVE ( )  GEOMETRIC_REPRESENTATION_ITEM ( )  RATIONAL_B_SPLINE_CURVE ( ( 0.9330127018922194093, 0.9330127018922194093, 1.000000000000000000, 0.8660254037844387076, 1.000000000000000000, 0.8660254037844387076, 1.000000000000000000, 0.9330127018922194093, 0.9330127018922194093 ) ) 
 REPRESENTATION_ITEM ( '' )  );
#4918 = CARTESIAN_POINT ( 'NONE',  ( -61.99999999999998579, 16.00000000000000000, 1.500000000000002220 ) ) ;
#4919 = CIRCLE ( 'NONE', #1385, 0.5999999999999999778 ) ;
#4920 = CARTESIAN_POINT ( 'NONE',  ( -120.0000000000000000, 3.999999999999980904, -2.000000000000000000 ) ) ;
#4921 = EDGE_LOOP ( 'NONE', ( #3034, #7353, #9276, #405 ) ) ;
#4922 = PLANE ( 'NONE',  #2476 ) ;
#4923 = ADVANCED_FACE ( 'NONE', ( #5835 ), #8346, .F. ) ;
#4924 = EDGE_CURVE ( 'NONE', #8323, #3410, #3882, .T. ) ;
#4925 = ORIENTED_EDGE ( 'NONE', *, *, #3272, .F. ) ;
#4926 = CARTESIAN_POINT ( 'NONE',  ( -60.99999999999998579, 9.489583332650536107, 0.9226497308103762673 ) ) ;
#4927 = CARTESIAN_POINT ( 'NONE',  ( -62.99999999999998579, 10.64583333333333570, 2.077350269189627952 ) ) ;
#4928 = VECTOR ( 'NONE', #3946, 1000.000000000000000 ) ;
#4929 = DIRECTION ( 'NONE',  ( -1.000000000000000000, -3.965082230804130220E-16, 0.000000000000000000 ) ) ;
#4930 = FACE_OUTER_BOUND ( 'NONE', #10250, .T. ) ;
#4931 = CARTESIAN_POINT ( 'NONE',  ( -61.49999999999998579, 9.010416665983868256, 0.6339745962155628467 ) ) ;
#4932 = VECTOR ( 'NONE', #1286, 1000.000000000000000 ) ;
#4933 = CARTESIAN_POINT ( 'NONE',  ( -62.43234176562499016, 11.30729166632526805, 2.248837904296538071 ) ) ;
#4934 = LINE ( 'NONE', #7343, #9625 ) ;
#4935 = ORIENTED_EDGE ( 'NONE', *, *, #8501, .T. ) ;
#4936 = DIRECTION ( 'NONE',  ( -0.000000000000000000, -0.000000000000000000, -1.000000000000000000 ) ) ;
#4937 = VECTOR ( 'NONE', #761, 1000.000000000000000 ) ;
#4938 = VERTEX_POINT ( 'NONE', #4160 ) ;
#4939 = CARTESIAN_POINT ( 'NONE',  ( 1.299999999999999156, 0.000000000000000000, 0.000000000000000000 ) ) ;
#4940 = CARTESIAN_POINT ( 'NONE',  ( -61.56765823437498142, 13.86979166632526805, 0.7511620957034663704 ) ) ;
#4941 = CONICAL_SURFACE ( 'NONE', #5824, 1.000000000000000888, 1.029744259999999967 ) ;
#4942 = CARTESIAN_POINT ( 'NONE',  ( 145.0000000000000284, -5.500000000000000000, 6.000000000000000000 ) ) ;
#4943 = FILL_AREA_STYLE ('',( #10741 ) ) ;
#4944 = CARTESIAN_POINT ( 'NONE',  ( -62.49999999999998579, 8.385416665983870033, 2.366025403784441483 ) ) ;
#4945 = CARTESIAN_POINT ( 'NONE',  ( -62.43234176562498305, 12.97395833299193590, 0.7511620957034662593 ) ) ;
#4946 = EDGE_CURVE ( 'NONE', #10494, #2251, #8991, .T. ) ;
#4947 = CARTESIAN_POINT ( 'NONE',  ( -61.99999999999998579, 14.95312499965860198, 0.5015494609379544944 ) ) ;
#4948 =( GEOMETRIC_REPRESENTATION_CONTEXT ( 3 ) GLOBAL_UNCERTAINTY_ASSIGNED_CONTEXT ( ( #8082 ) ) GLOBAL_UNIT_ASSIGNED_CONTEXT ( ( #7930, #7704, #256 ) ) REPRESENTATION_CONTEXT ( 'NONE', 'WORKASPACE' ) );
#4949 = DIRECTION ( 'NONE',  ( 0.000000000000000000, 1.000000000000000000, -0.000000000000000000 ) ) ;
#4950 = APPLICATION_PROTOCOL_DEFINITION ( 'draft international standard', 'automotive_design', 1998, #5555 ) ;
#4951 = LINE ( 'NONE', #9024, #154 ) ;
#4952 = CARTESIAN_POINT ( 'NONE',  ( -61.13531646874998415, 8.140624999658601979, 1.500000000000002220 ) ) ;
#4953 = CARTESIAN_POINT ( 'NONE',  ( -62.99999999999998579, 10.39583333333333393, 2.077350269189627952 ) ) ;
#4954 = VERTEX_POINT ( 'NONE', #3176 ) ;
#4955 = PLANE ( 'NONE',  #3188 ) ;
#4956 = CARTESIAN_POINT ( 'NONE',  ( 0.2300425840023376800, 0.2499999999999998335, -1.812072026511089229 ) ) ;
#4957 = VECTOR ( 'NONE', #7650, 1000.000000000000000 ) ;
#4958 = CARTESIAN_POINT ( 'NONE',  ( -61.13531646874997705, 14.34895833299193413, 1.000774730468978468 ) ) ;
#4959 = CARTESIAN_POINT ( 'NONE',  ( -62.86468353124998032, 10.18229166632526805, 1.000774730468978246 ) ) ;
#4960 = CARTESIAN_POINT ( 'NONE',  ( -61.13531646874997705, 15.61979166632526628, 1.999225269531026417 ) ) ;
#4961 = PLANE ( 'NONE',  #5872 ) ;
#4962 = VERTEX_POINT ( 'NONE', #5780 ) ;
#4963 = CARTESIAN_POINT ( 'NONE',  ( -61.49999999999998579, 13.29166666666666607, 0.6339745962155628467 ) ) ;
#4964 = CARTESIAN_POINT ( 'NONE',  ( -61.56765823437498852, 8.848958332991934128, 2.248837904296538515 ) ) ;
#4965 = VECTOR ( 'NONE', #725, 1000.000000000000000 ) ;
#4966 = CARTESIAN_POINT ( 'NONE',  ( -61.49999999999998579, 11.92708333265053611, 2.366025403784441927 ) ) ;
#4967 = CARTESIAN_POINT ( 'NONE',  ( -105.0000000000000000, 2.500000000000000000, 4.000000000000000000 ) ) ;
#4968 = FACE_OUTER_BOUND ( 'NONE', #4650, .T. ) ;
#4969 = CARTESIAN_POINT ( 'NONE',  ( -62.86468353124999453, 13.70312499965860198, 1.500000000000002220 ) ) ;
#4970 = CARTESIAN_POINT ( 'NONE',  ( -61.49999999999998579, 11.54166666666666785, 0.6339745962155628467 ) ) ;
#4971 = ORIENTED_EDGE ( 'NONE', *, *, #5725, .F. ) ;
#4972 = CARTESIAN_POINT ( 'NONE',  ( -62.43234176562498305, 12.97395833299193590, 0.7511620957034662593 ) ) ;
#4973 = FACE_OUTER_BOUND ( 'NONE', #2154, .T. ) ;
#4974 = PLANE ( 'NONE',  #346 ) ;
#4975 = APPLICATION_CONTEXT ( 'automotive_design' ) ;
#4976 = VERTEX_POINT ( 'NONE', #3126 ) ;
#4977 =( BOUNDED_CURVE ( )  B_SPLINE_CURVE ( 2, ( #5569, #10393, #8085, #2966, #7186, #8134, #2853, #10452, #3619 ),
 .UNSPECIFIED., .F., .T. ) 
 B_SPLINE_CURVE_WITH_KNOTS ( ( 3, 2, 2, 2, 3 ),
 ( 0.9609375000000000000, 0.9635416666666666297, 0.9687500000000000000, 0.9739583333333333703, 0.9765625000000000000 ),
 .UNSPECIFIED. ) 
 CURVE ( )  GEOMETRIC_REPRESENTATION_ITEM ( )  RATIONAL_B_SPLINE_CURVE ( ( 0.9330127018922194093, 0.9330127018922194093, 1.000000000000000000, 0.8660254037844387076, 1.000000000000000000, 0.8660254037844387076, 1.000000000000000000, 0.9330127018922194093, 0.9330127018922194093 ) ) 
 REPRESENTATION_ITEM ( '' )  );
#4978 = ORIENTED_EDGE ( 'NONE', *, *, #8825, .F. ) ;
#4979 = CARTESIAN_POINT ( 'NONE',  ( -134.9999999999999147, 10.63932022500203267, 3.000000000000000000 ) ) ;
#4980 = AXIS2_PLACEMENT_3D ( 'NONE', #70, #1738, #5112 ) ;
#4981 = CARTESIAN_POINT ( 'NONE',  ( -62.99999999999998579, 11.39583333333333393, 2.077350269189627952 ) ) ;
#4982 = ORIENTED_EDGE ( 'NONE', *, *, #1807, .F. ) ;
#4983 = CARTESIAN_POINT ( 'NONE',  ( -114.9999999999999147, -43.00000000000000000, -2.000000000000000000 ) ) ;
#4984 = CARTESIAN_POINT ( 'NONE',  ( -61.13531646874998415, 13.16145833299193413, 1.000774730468978468 ) ) ;
#4985 = EDGE_CURVE ( 'NONE', #9045, #7720, #6582, .T. ) ;
#4986 = DIRECTION ( 'NONE',  ( 1.000000000000000000, 0.000000000000000000, 0.000000000000000000 ) ) ;
#4987 = ORIENTED_EDGE ( 'NONE', *, *, #1929, .T. ) ;
#4988 = CLOSED_SHELL ( 'NONE', ( #6211, #1678, #1507, #6707, #9980, #3932, #3940, #7044, #6382, #8331, #7429, #9732, #8443, #503, #1219, #8713, #247, #9188, #3358, #6497 ) ) ;
#4989 = CARTESIAN_POINT ( 'NONE',  ( -61.73205080756888208, 10.91741454900183328, 2.500000000000006661 ) ) ;
#4990 = EDGE_LOOP ( 'NONE', ( #2927, #10193, #4195, #4788 ) ) ;
#4991 = CARTESIAN_POINT ( 'NONE',  ( -61.99999999999998579, 15.76562499965860020, 2.498450539062049724 ) ) ;
#4992 = CARTESIAN_POINT ( 'NONE',  ( -77.99999999999998579, -11.50000000000000711, 5.000000000000000000 ) ) ;
#4993 = CARTESIAN_POINT ( 'NONE',  ( -114.9999999999999289, -7.999999999999998224, -2.000000000000000000 ) ) ;
#4994 = DIRECTION ( 'NONE',  ( 0.000000000000000000, 1.000000000000000000, 0.000000000000000000 ) ) ;
#4995 = AXIS2_PLACEMENT_3D ( 'NONE', #2109, #7890, #8002 ) ;
#4996 = CARTESIAN_POINT ( 'NONE',  ( -61.56765823437498142, 12.93229166632526805, 0.7511620957034663704 ) ) ;
#4997 = VECTOR ( 'NONE', #3736, 1000.000000000000000 ) ;
#4998 = CARTESIAN_POINT ( 'NONE',  ( -62.43234176562499016, 15.80729166632526628, 2.248837904296538071 ) ) ;
#4999 = CARTESIAN_POINT ( 'NONE',  ( -61.49999999999998579, 14.95833333333333393, 2.366025403784441927 ) ) ;
#5000 = FACE_OUTER_BOUND ( 'NONE', #6134, .T. ) ;
#5001 = CARTESIAN_POINT ( 'NONE',  ( -62.86468353124998032, 8.994791666325268054, 1.000774730468978246 ) ) ;
#5002 = CARTESIAN_POINT ( 'NONE',  ( -105.0000000000000000, 2.500000000000000000, 4.000000000000000000 ) ) ;
#5003 = ORIENTED_EDGE ( 'NONE', *, *, #7226, .T. ) ;
#5004 = CARTESIAN_POINT ( 'NONE',  ( -61.99999999999998579, 11.78124999931720218, 0.5000000000000013323 ) ) ;
#5005 = CARTESIAN_POINT ( 'NONE',  ( -77.99999999999998579, 11.49999999999999645, 8.000000000000000000 ) ) ;
#5006 = CIRCLE ( 'NONE', #10326, 0.9999999999999983347 ) ;
#5007 = EDGE_CURVE ( 'NONE', #4740, #8859, #6523, .T. ) ;
#5008 = VECTOR ( 'NONE', #1259, 1000.000000000000000 ) ;
#5009 = CARTESIAN_POINT ( 'NONE',  ( -62.86468353124999453, 14.45312499965860020, 1.500000000000002220 ) ) ;
#5010 = CARTESIAN_POINT ( 'NONE',  ( -62.43234176562498305, 11.66145833299193590, 0.7511620957034662593 ) ) ;
#5011 = CARTESIAN_POINT ( 'NONE',  ( -61.56765823437498142, 15.18229166632526805, 0.7511620957034663704 ) ) ;
#5012 = CARTESIAN_POINT ( 'NONE',  ( -61.99999999999998579, 9.656249999317202182, 2.500000000000002665 ) ) ;
#5013 = ORIENTED_EDGE ( 'NONE', *, *, #3692, .F. ) ;
#5014 = CARTESIAN_POINT ( 'NONE',  ( -60.99999999999998579, 13.97916666666666785, 2.077350269189628840 ) ) ;
#5015 = CARTESIAN_POINT ( 'NONE',  ( -61.13531646874997705, 8.911458332991934128, 1.000774730468978468 ) ) ;
#5016 = SHAPE_REPRESENTATION ( 'stationary jaw', ( #2307 ), #3714 ) ;
#5017 =( NAMED_UNIT ( * ) PLANE_ANGLE_UNIT ( ) SI_UNIT ( $, .RADIAN. ) );
#5018 = VECTOR ( 'NONE', #8795, 1000.000000000000000 ) ;
#5019 = CARTESIAN_POINT ( 'NONE',  ( -62.99999999999998579, 11.61458333265053611, 2.077350269189627952 ) ) ;
#5020 = ORIENTED_EDGE ( 'NONE', *, *, #677, .T. ) ;
#5021 = CARTESIAN_POINT ( 'NONE',  ( -60.99999999999998579, 9.500000000000000000, 1.500000000000002220 ) ) ;
#5022 = VECTOR ( 'NONE', #6677, 1000.000000000000000 ) ;
#5023 = CARTESIAN_POINT ( 'NONE',  ( -61.99999999999998579, 13.51562499965860198, 2.498450539062049724 ) ) ;
#5024 = CARTESIAN_POINT ( 'NONE',  ( -61.99999999999998579, 14.43749999999999822, 2.500000000000002665 ) ) ;
#5025 = ORIENTED_EDGE ( 'NONE', *, *, #2419, .T. ) ;
#5026 = CARTESIAN_POINT ( 'NONE',  ( -61.13531646874998415, 13.14062499965860198, 1.500000000000002220 ) ) ;
#5027 = CARTESIAN_POINT ( 'NONE',  ( -60.99999999999998579, 11.48958333265053611, 0.9226497308103762673 ) ) ;
#5028 = LINE ( 'NONE', #1654, #8164 ) ;
#5029 = ORIENTED_EDGE ( 'NONE', *, *, #10336, .F. ) ;
#5030 = CARTESIAN_POINT ( 'NONE',  ( -62.26794919243111082, 12.42633545031537068, 2.500000000000003109 ) ) ;
#5031 = EDGE_CURVE ( 'NONE', #8575, #5931, #8274, .T. ) ;
#5032 = VERTEX_POINT ( 'NONE', #7510 ) ;
#5033 = CARTESIAN_POINT ( 'NONE',  ( -60.99999999999998579, 10.75000000000000000, 1.500000000000002220 ) ) ;
#5034 = VERTEX_POINT ( 'NONE', #10892 ) ;
#5035 = CARTESIAN_POINT ( 'NONE',  ( -62.86468353124999453, 8.265624999658601979, 1.500000000000002220 ) ) ;
#5036 = CARTESIAN_POINT ( 'NONE',  ( -99.99999999999995737, -12.99999999999998757, 0.000000000000000000 ) ) ;
#5037 = ADVANCED_FACE ( 'NONE', ( #7616 ), #3606, .F. ) ;
#5038 = CARTESIAN_POINT ( 'NONE',  ( -61.13531646874998415, 12.86979166632526628, 1.999225269531026417 ) ) ;
#5039 = CARTESIAN_POINT ( 'NONE',  ( -60.99999999999998579, 13.27083333333333215, 0.9226497308103762673 ) ) ;
#5040 = VERTEX_POINT ( 'NONE', #105 ) ;
#5041 = DIRECTION ( 'NONE',  ( 1.000000000000000000, 1.110223024625156343E-15, -0.000000000000000000 ) ) ;
#5042 = ORIENTED_EDGE ( 'NONE', *, *, #3824, .F. ) ;
#5043 = CARTESIAN_POINT ( 'NONE',  ( -61.49999999999998579, 13.17708333265053433, 2.366025403784441927 ) ) ;
#5044 = CARTESIAN_POINT ( 'NONE',  ( -61.99999999999998579, 14.76562499965859843, 2.498450539062049724 ) ) ;
#5045 = DIRECTION ( 'NONE',  ( 0.000000000000000000, 0.000000000000000000, -1.000000000000000000 ) ) ;
#5046 = LINE ( 'NONE', #4317, #7967 ) ;
#5047 = CARTESIAN_POINT ( 'NONE',  ( -61.99999999999998579, 15.18750000000000000, 2.500000000000002665 ) ) ;
#5048 = CARTESIAN_POINT ( 'NONE',  ( -62.86468353124999453, 12.53645833299193413, 1.999225269531025750 ) ) ;
#5049 = CARTESIAN_POINT ( 'NONE',  ( -62.86468353124998742, 15.78645833299193590, 1.999225269531025972 ) ) ;
#5050 = CYLINDRICAL_SURFACE ( 'NONE', #4053, 0.9999999999999981126 ) ;
#5051 = CARTESIAN_POINT ( 'NONE',  ( 1.299999999999999156, 0.000000000000000000, 0.000000000000000000 ) ) ;
#5052 = CARTESIAN_POINT ( 'NONE',  ( -61.99999999999998579, 9.453124999658600203, 0.5015494609379544944 ) ) ;
#5053 =( REPRESENTATION_RELATIONSHIP ('NONE','NONE', #560, #2752 ) REPRESENTATION_RELATIONSHIP_WITH_TRANSFORMATION ( #10013 )SHAPE_REPRESENTATION_RELATIONSHIP( ) );
#5054 = DIRECTION ( 'NONE',  ( 0.000000000000000000, 0.000000000000000000, -1.000000000000000000 ) ) ;
#5055 = ORIENTED_EDGE ( 'NONE', *, *, #4052, .F. ) ;
#5056 = DIRECTION ( 'NONE',  ( 0.000000000000000000, -1.000000000000000000, 0.000000000000000000 ) ) ;
#5057 = CARTESIAN_POINT ( 'NONE',  ( -61.99999999999998579, 14.99999999999998579, 1.500000000000002220 ) ) ;
#5058 = EDGE_CURVE ( 'NONE', #7983, #2258, #5151, .T. ) ;
#5059 = CARTESIAN_POINT ( 'NONE',  ( -62.86468353124999453, 15.22395833299193590, 1.999225269531025750 ) ) ;
#5060 = CARTESIAN_POINT ( 'NONE',  ( -61.13531646874998415, 11.59895833299193590, 1.000774730468978468 ) ) ;
#5061 = EDGE_CURVE ( 'NONE', #1608, #10509, #1746, .T. ) ;
#5062 = CARTESIAN_POINT ( 'NONE',  ( -62.86468353124999453, 15.53645833299193590, 1.999225269531025750 ) ) ;
#5063 = CYLINDRICAL_SURFACE ( 'NONE', #10127, 2.500000000000002220 ) ;
#5064 = ORIENTED_EDGE ( 'NONE', *, *, #8342, .T. ) ;
#5065 = CARTESIAN_POINT ( 'NONE',  ( -61.49999999999998579, 15.20833333333333393, 2.366025403784441927 ) ) ;
#5066 = CARTESIAN_POINT ( 'NONE',  ( -61.13531646874997705, 8.619791666325268054, 1.999225269531026417 ) ) ;
#5067 = CARTESIAN_POINT ( 'NONE',  ( -61.99999999999998579, 12.65624999931720396, 2.654700538379254571 ) ) ;
#5068 = EDGE_LOOP ( 'NONE', ( #10141, #3484, #5649, #7977 ) ) ;
#5069 = CYLINDRICAL_SURFACE ( 'NONE', #9820, 0.9999999999999981126 ) ;
#5070 = CARTESIAN_POINT ( 'NONE',  ( -61.99999999999999289, 12.14062499965860198, 0.5015494609379544944 ) ) ;
#5071 = DIRECTION ( 'NONE',  ( -0.000000000000000000, -0.000000000000000000, -1.000000000000000000 ) ) ;
#5072 = EDGE_LOOP ( 'NONE', ( #6097, #4935 ) ) ;
#5073 = DIRECTION ( 'NONE',  ( -1.000000000000000000, -2.478176394252581696E-17, 0.000000000000000000 ) ) ;
#5074 = CARTESIAN_POINT ( 'NONE',  ( -62.86468353124999453, 12.76562499965860198, 1.500000000000002220 ) ) ;
#5075 = DIRECTION ( 'NONE',  ( 0.000000000000000000, 0.000000000000000000, -1.000000000000000000 ) ) ;
#5076 = EDGE_CURVE ( 'NONE', #2754, #947, #7775, .T. ) ;
#5077 = EDGE_LOOP ( 'NONE', ( #3557, #669, #3876, #1133 ) ) ;
#5078 = CARTESIAN_POINT ( 'NONE',  ( -61.99999999999998579, 12.18749999999999822, 2.500000000000002665 ) ) ;
#5079 = ORIENTED_EDGE ( 'NONE', *, *, #4533, .T. ) ;
#5080 = LINE ( 'NONE', #9264, #4792 ) ;
#5081 = ORIENTED_EDGE ( 'NONE', *, *, #10917, .T. ) ;
#5082 = ORIENTED_EDGE ( 'NONE', *, *, #703, .T. ) ;
#5083 = CARTESIAN_POINT ( 'NONE',  ( -61.56765823437498852, 9.348958332991935904, 2.248837904296538515 ) ) ;
#5084 = EDGE_CURVE ( 'NONE', #7919, #2018, #9494, .T. ) ;
#5085 = CARTESIAN_POINT ( 'NONE',  ( -62.86468353124998032, 12.99479166632526805, 1.000774730468978246 ) ) ;
#5086 = CARTESIAN_POINT ( 'NONE',  ( -62.99999999999998579, 12.11458333265053611, 2.077350269189627952 ) ) ;
#5087 = VERTEX_POINT ( 'NONE', #7004 ) ;
#5088 = DIRECTION ( 'NONE',  ( -1.000000000000000000, 0.000000000000000000, -0.000000000000000000 ) ) ;
#5089 =( GEOMETRIC_REPRESENTATION_CONTEXT ( 3 ) GLOBAL_UNCERTAINTY_ASSIGNED_CONTEXT ( ( #5822 ) ) GLOBAL_UNIT_ASSIGNED_CONTEXT ( ( #2318, #650, #1646 ) ) REPRESENTATION_CONTEXT ( 'NONE', 'WORKASPACE' ) );
#5090 = PRODUCT_DEFINITION_SHAPE ( 'NONE', 'NONE',  #932 ) ;
#5091 = EDGE_CURVE ( 'NONE', #3634, #5427, #5889, .T. ) ;
#5092 = ORIENTED_EDGE ( 'NONE', *, *, #985, .F. ) ;
#5093 = CYLINDRICAL_SURFACE ( 'NONE', #6078, 0.9999999999999981126 ) ;
#5094 = CARTESIAN_POINT ( 'NONE',  ( -61.13531646874998415, 15.82812499965860198, 1.500000000000002220 ) ) ;
#5095 = CARTESIAN_POINT ( 'NONE',  ( -61.99999999999998579, 16.00000000000000000, 2.500000000000000444 ) ) ;
#5096 = CARTESIAN_POINT ( 'NONE',  ( -60.99999999999998579, 12.50000000000000000, 1.500000000000002220 ) ) ;
#5097 = CARTESIAN_POINT ( 'NONE',  ( -61.99999999999997868, 10.68749999999999822, 2.500000000000002665 ) ) ;
#5098 = CARTESIAN_POINT ( 'NONE',  ( -62.43234176562499016, 12.80729166632526805, 2.248837904296538071 ) ) ;
#5099 = CARTESIAN_POINT ( 'NONE',  ( -61.56765823437498852, 9.036458332991935904, 2.248837904296538515 ) ) ;
#5100 = CYLINDRICAL_SURFACE ( 'NONE', #5111, 0.9999999999999981126 ) ;
#5101 = FACE_OUTER_BOUND ( 'NONE', #3845, .T. ) ;
#5102 = CARTESIAN_POINT ( 'NONE',  ( -62.86468353124998742, 8.786458332991934128, 1.999225269531025972 ) ) ;
#5103 = AXIS2_PLACEMENT_3D ( 'NONE', #6155, #9540, #1934 ) ;
#5104 = CARTESIAN_POINT ( 'NONE',  ( 146.0000000000000284, 5.500000000000000000, 3.000000000000000000 ) ) ;
#5105 = ORIENTED_EDGE ( 'NONE', *, *, #5807, .T. ) ;
#5106 = CARTESIAN_POINT ( 'NONE',  ( -61.99999999999998579, 12.03124999931720041, 0.5000000000000013323 ) ) ;
#5107 = CARTESIAN_POINT ( 'NONE',  ( -105.0000000000000000, -2.500000000000000000, 4.000000000000000000 ) ) ;
#5108 = CARTESIAN_POINT ( 'NONE',  ( -61.99999999999999289, 15.01562499965860020, 2.498450539062049724 ) ) ;
#5109 = CARTESIAN_POINT ( 'NONE',  ( -61.13531646874998415, 11.07812499965860020, 1.500000000000002220 ) ) ;
#5110 = CARTESIAN_POINT ( 'NONE',  ( -62.43234176562499016, 15.05729166632526805, 2.248837904296538071 ) ) ;
#5111 = AXIS2_PLACEMENT_3D ( 'NONE', #942, #5896, #5 ) ;
#5112 = DIRECTION ( 'NONE',  ( 1.000000000000000000, 0.000000000000000000, -0.000000000000000000 ) ) ;
#5113 = VERTEX_POINT ( 'NONE', #1889 ) ;
#5114 = CARTESIAN_POINT ( 'NONE',  ( -61.99999999999998579, 15.68750000000000000, 2.654700538379254571 ) ) ;
#5115 = CARTESIAN_POINT ( 'NONE',  ( -61.56765823437498142, 9.182291666325268054, 0.7511620957034663704 ) ) ;
#5116 = AXIS2_PLACEMENT_3D ( 'NONE', #3338, #5269, #999 ) ;
#5117 = CARTESIAN_POINT ( 'NONE',  ( -60.99999999999998579, 13.21874999931720396, 1.500000000000002220 ) ) ;
#5118 = CARTESIAN_POINT ( 'NONE',  ( 150.0000000000000000, -8.000000000000000000, 3.000000000000000000 ) ) ;
#5119 = ORIENTED_EDGE ( 'NONE', *, *, #5084, .F. ) ;
#5120 = DIRECTION ( 'NONE',  ( -2.478176394252581696E-17, 1.000000000000000000, 0.000000000000000000 ) ) ;
#5121 = EDGE_CURVE ( 'NONE', #1296, #4198, #8555, .T. ) ;
#5122 = PRESENTATION_LAYER_ASSIGNMENT (  '', '', ( #9935 ) ) ;
#5123 = CARTESIAN_POINT ( 'NONE',  ( -61.13531646874998415, 11.57812499965860198, 1.500000000000002220 ) ) ;
#5124 = DIRECTION ( 'NONE',  ( -0.000000000000000000, -0.000000000000000000, 1.000000000000000000 ) ) ;
#5125 = VECTOR ( 'NONE', #8185, 1000.000000000000000 ) ;
#5126 = ORIENTED_EDGE ( 'NONE', *, *, #6868, .F. ) ;
#5127 = CARTESIAN_POINT ( 'NONE',  ( -61.99999999999998579, 12.81250000000000000, 0.5000000000000013323 ) ) ;
#5128 = CARTESIAN_POINT ( 'NONE',  ( -61.13531646874998415, 13.39062499965860020, 1.500000000000002220 ) ) ;
#5129 =( NAMED_UNIT ( * ) PLANE_ANGLE_UNIT ( ) SI_UNIT ( $, .RADIAN. ) );
#5130 = LINE ( 'NONE', #913, #9370 ) ;
#5131 = CARTESIAN_POINT ( 'NONE',  ( -62.49999999999998579, 9.802083332650536107, 0.6339745962155627357 ) ) ;
#5132 = ORIENTED_EDGE ( 'NONE', *, *, #9294, .F. ) ;
#5133 = CARTESIAN_POINT ( 'NONE',  ( -61.99999999999998579, 13.93749999999999822, 2.500000000000002665 ) ) ;
#5134 = ORIENTED_EDGE ( 'NONE', *, *, #3278, .F. ) ;
#5135 = FACE_OUTER_BOUND ( 'NONE', #1217, .T. ) ;
#5136 =( BOUNDED_CURVE ( )  B_SPLINE_CURVE ( 2, ( #3312, #9313, #10138, #6872, #10246, #2654, #2539, #5030, #10088 ),
 .UNSPECIFIED., .F., .T. ) 
 B_SPLINE_CURVE_WITH_KNOTS ( ( 3, 2, 2, 2, 3 ),
 ( 0.5390625000000000000, 0.5416666666666666297, 0.5468750000000000000, 0.5520833333333333703, 0.5546875000000000000 ),
 .UNSPECIFIED. ) 
 CURVE ( )  GEOMETRIC_REPRESENTATION_ITEM ( )  RATIONAL_B_SPLINE_CURVE ( ( 0.9330127018922194093, 0.9330127018922194093, 1.000000000000000000, 0.8660254037844387076, 1.000000000000000000, 0.8660254037844387076, 1.000000000000000000, 0.9330127018922194093, 0.9330127018922194093 ) ) 
 REPRESENTATION_ITEM ( '' )  );
#5137 = CARTESIAN_POINT ( 'NONE',  ( -61.99999999999998579, 11.51562499965860020, 2.498450539062049724 ) ) ;
#5138 = ADVANCED_FACE ( 'NONE', ( #7836 ), #7781, .F. ) ;
#5139 = SURFACE_STYLE_USAGE ( .BOTH. , #3533 ) ;
#5140 = ORIENTED_EDGE ( 'NONE', *, *, #3045, .F. ) ;
#5141 = CARTESIAN_POINT ( 'NONE',  ( -61.13531646874998415, 9.119791666325268054, 1.999225269531026417 ) ) ;
#5142 = DIRECTION ( 'NONE',  ( -1.000000000000000000, 0.000000000000000000, 0.000000000000000000 ) ) ;
#5143 = PRODUCT_CONTEXT ( 'NONE', #10872, 'mechanical' ) ;
#5144 = CARTESIAN_POINT ( 'NONE',  ( -61.56765823437498142, 12.93229166632526805, 0.7511620957034663704 ) ) ;
#5145 = CARTESIAN_POINT ( 'NONE',  ( -62.26794919243111082, 12.14508544963257464, 2.500000000000003109 ) ) ;
#5146 = ORIENTED_EDGE ( 'NONE', *, *, #9135, .F. ) ;
#5147 = DIRECTION ( 'NONE',  ( 0.7071067811865463515, 8.659560562354918067E-17, -0.7071067811865487940 ) ) ;
#5148 = ORIENTED_EDGE ( 'NONE', *, *, #10172, .F. ) ;
#5149 = CARTESIAN_POINT ( 'NONE',  ( -61.56765823437498852, 14.78645833299193413, 2.248837904296538515 ) ) ;
#5150 = CARTESIAN_POINT ( 'NONE',  ( -43.00000000000000000, -14.00000000000000888, -2.000000000000000000 ) ) ;
#5151 = LINE ( 'NONE', #1, #9368 ) ;
#5152 = CARTESIAN_POINT ( 'NONE',  ( -62.49999999999998579, 12.38541666598386826, 2.366025403784441483 ) ) ;
#5153 = CARTESIAN_POINT ( 'NONE',  ( -61.13531646874997705, 13.61979166632526983, 1.999225269531026417 ) ) ;
#5154 = CARTESIAN_POINT ( 'NONE',  ( -61.13531646874998415, 9.328124999658600203, 1.500000000000002220 ) ) ;
#5155 = LINE ( 'NONE', #10212, #9041 ) ;
#5156 = CYLINDRICAL_SURFACE ( 'NONE', #1931, 0.9999999999999981126 ) ;
#5157 = CARTESIAN_POINT ( 'NONE',  ( -62.86468353124998742, 9.036458332991934128, 1.999225269531025972 ) ) ;
#5158 = CARTESIAN_POINT ( 'NONE',  ( -60.99999999999998579, 15.73958333265053788, 0.9226497308103762673 ) ) ;
#5159 = ORIENTED_EDGE ( 'NONE', *, *, #1993, .T. ) ;
#5160 = CARTESIAN_POINT ( 'NONE',  ( -114.9999999999999289, -8.000000000000000000, 3.000000000000000000 ) ) ;
#5161 = CARTESIAN_POINT ( 'NONE',  ( 143.9000000000000341, 5.500000000000000000, 3.000000000000000888 ) ) ;
#5162 = CARTESIAN_POINT ( 'NONE',  ( -62.43234176562498305, 15.16145833299193590, 0.7511620957034662593 ) ) ;
#5163 = CARTESIAN_POINT ( 'NONE',  ( -61.13531646874998415, 11.05729166632526805, 1.999225269531026417 ) ) ;
#5164 = CARTESIAN_POINT ( 'NONE',  ( -61.99999999999999289, 8.640624999658601979, 0.5015494609379544944 ) ) ;
#5165 = SURFACE_STYLE_FILL_AREA ( #9510 ) ;
#5166 = ORIENTED_EDGE ( 'NONE', *, *, #3313, .T. ) ;
#5167 = CARTESIAN_POINT ( 'NONE',  ( -62.99999999999998579, 14.89583333333333570, 2.077350269189627952 ) ) ;
#5168 = CARTESIAN_POINT ( 'NONE',  ( -61.13531646874997705, 8.869791666325268054, 1.999225269531026417 ) ) ;
#5169 = EDGE_CURVE ( 'NONE', #8097, #1119, #1837, .T. ) ;
#5170 = CARTESIAN_POINT ( 'NONE',  ( -62.49999999999998579, 12.63541666598386826, 2.366025403784441483 ) ) ;
#5171 = CARTESIAN_POINT ( 'NONE',  ( -61.99999999999998579, 13.06250000000000178, 0.5000000000000013323 ) ) ;
#5172 = VECTOR ( 'NONE', #1343, 1000.000000000000000 ) ;
#5173 = CARTESIAN_POINT ( 'NONE',  ( -62.26794919243111082, 11.67633545031536890, 2.500000000000003109 ) ) ;
#5174 = CARTESIAN_POINT ( 'NONE',  ( -61.13531646874997705, 11.34895833299193413, 1.000774730468978468 ) ) ;
#5175 = CARTESIAN_POINT ( 'NONE',  ( 145.0000000000000284, 5.500000000000000000, 6.000000000000000000 ) ) ;
#5176 = CARTESIAN_POINT ( 'NONE',  ( -57.99999999999998579, -14.00000000000001243, 3.000000000000000000 ) ) ;
#5177 = ORIENTED_EDGE ( 'NONE', *, *, #10324, .T. ) ;
#5178 = VECTOR ( 'NONE', #2402, 1000.000000000000000 ) ;
#5179 = CARTESIAN_POINT ( 'NONE',  ( -57.99999999999998579, -14.00000000000001243, 0.000000000000000000 ) ) ;
#5180 = EDGE_CURVE ( 'NONE', #8943, #9934, #5046, .T. ) ;
#5181 = CARTESIAN_POINT ( 'NONE',  ( -62.43234176562499016, 13.05729166632526805, 2.248837904296538071 ) ) ;
#5182 =( NAMED_UNIT ( * ) PLANE_ANGLE_UNIT ( ) SI_UNIT ( $, .RADIAN. ) );
#5183 = DIRECTION ( 'NONE',  ( -0.000000000000000000, -1.000000000000000000, -0.000000000000000000 ) ) ;
#5184 = CARTESIAN_POINT ( 'NONE',  ( -62.49999999999998579, 9.552083332650536107, 0.6339745962155627357 ) ) ;
#5185 = ORIENTED_EDGE ( 'NONE', *, *, #9918, .F. ) ;
#5186 = PRODUCT ( 'dial indicator', 'dial indicator', '', ( #10690 ) ) ;
#5187 = CARTESIAN_POINT ( 'NONE',  ( -61.99999999999998579, 13.43749999999999822, 2.500000000000002665 ) ) ;
#5188 = ORIENTED_EDGE ( 'NONE', *, *, #1154, .T. ) ;
#5189 = CIRCLE ( 'NONE', #1833, 30.00000000000000000 ) ;
#5190 = LINE ( 'NONE', #4351, #6219 ) ;
#5191 = CARTESIAN_POINT ( 'NONE',  ( -61.99999999999998579, 11.89062499965860198, 0.5015494609379544944 ) ) ;
#5192 = EDGE_CURVE ( 'NONE', #24, #7065, #3549, .T. ) ;
#5193 = CARTESIAN_POINT ( 'NONE',  ( 0.000000000000000000, 0.000000000000000000, 0.000000000000000000 ) ) ;
#5194 = ORIENTED_EDGE ( 'NONE', *, *, #2918, .T. ) ;
#5195 = EDGE_CURVE ( 'NONE', #5268, #4846, #8623, .T. ) ;
#5196 = CARTESIAN_POINT ( 'NONE',  ( -62.86468353124999453, 9.015624999658601979, 1.500000000000002220 ) ) ;
#5197 = CARTESIAN_POINT ( 'NONE',  ( -62.49999999999998579, 13.80208333265053611, 0.6339745962155627357 ) ) ;
#5198 = EDGE_CURVE ( 'NONE', #3585, #4054, #10207, .T. ) ;
#5199 = CARTESIAN_POINT ( 'NONE',  ( -62.43234176562498305, 12.72395833299193413, 0.7511620957034662593 ) ) ;
#5200 = CARTESIAN_POINT ( 'NONE',  ( -104.9999999999999289, -7.999999999999994671, 0.000000000000000000 ) ) ;
#5201 = ORIENTED_EDGE ( 'NONE', *, *, #7114, .T. ) ;
#5202 =( BOUNDED_CURVE ( )  B_SPLINE_CURVE ( 2, ( #2496, #6831, #10202, #10375, #7169, #8895, #9604, #8657, #2835 ),
 .UNSPECIFIED., .F., .T. ) 
 B_SPLINE_CURVE_WITH_KNOTS ( ( 3, 2, 2, 2, 3 ),
 ( 0.1640624999999999722, 0.1666666666666666574, 0.1718750000000000000, 0.1770833333333333426, 0.1796875000000000000 ),
 .UNSPECIFIED. ) 
 CURVE ( )  GEOMETRIC_REPRESENTATION_ITEM ( )  RATIONAL_B_SPLINE_CURVE ( ( 0.9330127018922194093, 0.9330127018922186322, 1.000000000000000000, 0.8660254037844387076, 1.000000000000000000, 0.8660254037844387076, 1.000000000000000000, 0.9330127018922194093, 0.9330127018922194093 ) ) 
 REPRESENTATION_ITEM ( '' )  );
#5203 = DIRECTION ( 'NONE',  ( -1.000000000000000000, 0.000000000000000000, 0.000000000000000000 ) ) ;
#5204 = EDGE_LOOP ( 'NONE', ( #3100, #448, #10962, #10666 ) ) ;
#5205 = CARTESIAN_POINT ( 'NONE',  ( -62.99999999999998579, 11.59374999931720218, 1.500000000000001998 ) ) ;
#5206 = CARTESIAN_POINT ( 'NONE',  ( -61.13531646874998415, 15.05729166632526805, 1.999225269531026417 ) ) ;
#5207 = FACE_OUTER_BOUND ( 'NONE', #6819, .T. ) ;
#5208 = DIRECTION ( 'NONE',  ( -0.000000000000000000, -0.000000000000000000, -1.000000000000000000 ) ) ;
#5209 = PLANE ( 'NONE',  #5645 ) ;
#5210 = CARTESIAN_POINT ( 'NONE',  ( -62.86468353124999453, 13.76562499965860198, 1.500000000000002220 ) ) ;
#5211 = CARTESIAN_POINT ( 'NONE',  ( -62.86468353124999453, 8.203124999658601979, 1.500000000000002220 ) ) ;
#5212 = CARTESIAN_POINT ( 'NONE',  ( -120.0000000000000000, -4.000000000000019540, -2.000000000000000000 ) ) ;
#5213 = CARTESIAN_POINT ( 'NONE',  ( -61.99999999999998579, 15.78124999931720041, 0.5000000000000013323 ) ) ;
#5214 = CARTESIAN_POINT ( 'NONE',  ( -61.13531646874998415, 8.619791666325268054, 1.999225269531026417 ) ) ;
#5215 = CARTESIAN_POINT ( 'NONE',  ( -62.99999999999998579, 14.09374999931720218, 1.500000000000001998 ) ) ;
#5216 = EDGE_LOOP ( 'NONE', ( #1508, #4572 ) ) ;
#5217 = LINE ( 'NONE', #3447, #706 ) ;
#5218 = CARTESIAN_POINT ( 'NONE',  ( -62.86468353124998032, 15.93229166632526628, 1.000774730468978024 ) ) ;
#5219 = CARTESIAN_POINT ( 'NONE',  ( -61.13531646874998415, 11.34895833299193413, 1.000774730468978468 ) ) ;
#5220 = CARTESIAN_POINT ( 'NONE',  ( -62.86468353124998032, 8.682291666325268054, 1.000774730468978024 ) ) ;
#5221 = CARTESIAN_POINT ( 'NONE',  ( -62.99999999999998579, 13.07291666598386826, 0.9226497308103756012 ) ) ;
#5222 = VERTEX_POINT ( 'NONE', #3490 ) ;
#5223 = CARTESIAN_POINT ( 'NONE',  ( -62.49999999999998579, 14.91666666666666607, 2.366025403784441483 ) ) ;
#5224 = CARTESIAN_POINT ( 'NONE',  ( -61.13531646874997705, 10.36979166632526983, 1.999225269531026417 ) ) ;
#5225 = SURFACE_SIDE_STYLE ('',( #8466 ) ) ;
#5226 = CARTESIAN_POINT ( 'NONE',  ( -62.99999999999998579, 13.32291666598386826, 0.9226497308103756012 ) ) ;
#5227 = LINE ( 'NONE', #7748, #8762 ) ;
#5228 = ORIENTED_EDGE ( 'NONE', *, *, #5376, .F. ) ;
#5229 = EDGE_CURVE ( 'NONE', #4626, #4740, #2726, .T. ) ;
#5230 = DIRECTION ( 'NONE',  ( -0.000000000000000000, -0.000000000000000000, 1.000000000000000000 ) ) ;
#5231 = CARTESIAN_POINT ( 'NONE',  ( -61.99999999999999289, 11.39062499965859843, 0.5015494609379544944 ) ) ;
#5232 = EDGE_CURVE ( 'NONE', #3356, #8335, #2778, .T. ) ;
#5233 = CYLINDRICAL_SURFACE ( 'NONE', #2437, 1.000000000000000888 ) ;
#5234 = CARTESIAN_POINT ( 'NONE',  ( 0.5000000000000000000, -0.2499999999999997224, -2.000000000000000000 ) ) ;
#5235 = ORIENTED_EDGE ( 'NONE', *, *, #9211, .T. ) ;
#5236 = CARTESIAN_POINT ( 'NONE',  ( -61.49999999999998579, 10.95833333333333393, 2.366025403784441927 ) ) ;
#5237 = PLANE ( 'NONE',  #5549 ) ;
#5238 = CARTESIAN_POINT ( 'NONE',  ( -62.86468353124998032, 13.74479166632526805, 1.000774730468978246 ) ) ;
#5239 =( NAMED_UNIT ( * ) SI_UNIT ( $, .STERADIAN. ) SOLID_ANGLE_UNIT ( ) );
#5240 = CARTESIAN_POINT ( 'NONE',  ( 0.000000000000000000, -0.2499999999999999445, 1.312875263449798879 ) ) ;
#5241 = CARTESIAN_POINT ( 'NONE',  ( -61.49999999999998579, 8.760416665983868256, 0.6339745962155628467 ) ) ;
#5242 = ORIENTED_EDGE ( 'NONE', *, *, #4038, .F. ) ;
#5243 = CARTESIAN_POINT ( 'NONE',  ( -76.89999999999999147, -11.50000000000000711, -2.000000000000000000 ) ) ;
#5244 = PLANE ( 'NONE',  #8470 ) ;
#5245 = CARTESIAN_POINT ( 'NONE',  ( -62.43234176562498305, 11.66145833299193590, 0.7511620957034662593 ) ) ;
#5246 =( LENGTH_UNIT ( ) NAMED_UNIT ( * ) SI_UNIT ( .MILLI., .METRE. ) );
#5247 = VERTEX_POINT ( 'NONE', #6165 ) ;
#5248 = CARTESIAN_POINT ( 'NONE',  ( -61.56765823437498142, 9.182291666325268054, 0.7511620957034663704 ) ) ;
#5249 = LINE ( 'NONE', #7163, #5820 ) ;
#5250 = EDGE_CURVE ( 'NONE', #9380, #5859, #7174, .T. ) ;
#5251 = CARTESIAN_POINT ( 'NONE',  ( -62.86468353124998742, 14.28645833299193413, 1.999225269531025972 ) ) ;
#5252 = CARTESIAN_POINT ( 'NONE',  ( -61.99999999999998579, 12.15624999931720041, 2.500000000000002665 ) ) ;
#5253 = VERTEX_POINT ( 'NONE', #8839 ) ;
#5254 = EDGE_CURVE ( 'NONE', #6924, #7749, #8010, .T. ) ;
#5255 = VECTOR ( 'NONE', #5418, 1000.000000000000000 ) ;
#5256 = VERTEX_POINT ( 'NONE', #9670 ) ;
#5257 = FACE_OUTER_BOUND ( 'NONE', #5204, .T. ) ;
#5258 = CARTESIAN_POINT ( 'NONE',  ( -61.49999999999998579, 8.208333333333333925, 2.366025403784441927 ) ) ;
#5259 = DIRECTION ( 'NONE',  ( 0.000000000000000000, 0.000000000000000000, -1.000000000000000000 ) ) ;
#5260 = CARTESIAN_POINT ( 'NONE',  ( -105.0000000000000000, -2.500000000000000000, 4.000000000000000000 ) ) ;
#5261 = CARTESIAN_POINT ( 'NONE',  ( -104.9999999999999289, -16.54248688935409106, -2.000000000000000000 ) ) ;
#5262 = CARTESIAN_POINT ( 'NONE',  ( -62.86468353124999453, 13.78645833299193413, 1.999225269531025750 ) ) ;
#5263 = CARTESIAN_POINT ( 'NONE',  ( -61.13531646874998415, 8.848958332991935904, 1.000774730468978468 ) ) ;
#5264 = CARTESIAN_POINT ( 'NONE',  ( -60.99999999999998579, 9.250000000000000000, 1.500000000000002220 ) ) ;
#5265 = FACE_BOUND ( 'NONE', #10925, .T. ) ;
#5266 = CARTESIAN_POINT ( 'NONE',  ( -61.13531646874998415, 9.869791666325269830, 1.999225269531026417 ) ) ;
#5267 = CARTESIAN_POINT ( 'NONE',  ( 0.05011565059742434380, 0.2499999999999982792, -1.595010514166263382 ) ) ;
#5268 = VERTEX_POINT ( 'NONE', #7056 ) ;
#5269 = DIRECTION ( 'NONE',  ( 0.000000000000000000, 0.000000000000000000, -1.000000000000000000 ) ) ;
#5270 = CARTESIAN_POINT ( 'NONE',  ( -61.99999999999999289, 15.51562499965860198, 2.498450539062049724 ) ) ;
#5271 = EDGE_CURVE ( 'NONE', #2471, #9265, #4607, .T. ) ;
#5272 = CARTESIAN_POINT ( 'NONE',  ( -61.99999999999998579, 12.01562499965860020, 2.498450539062049724 ) ) ;
#5273 =( GEOMETRIC_REPRESENTATION_CONTEXT ( 3 ) GLOBAL_UNCERTAINTY_ASSIGNED_CONTEXT ( ( #3271 ) ) GLOBAL_UNIT_ASSIGNED_CONTEXT ( ( #2442, #1462, #4887 ) ) REPRESENTATION_CONTEXT ( 'NONE', 'WORKASPACE' ) );
#5274 = CARTESIAN_POINT ( 'NONE',  ( -62.86468353124999453, 8.953124999658601979, 1.500000000000002220 ) ) ;
#5275 = DIRECTION ( 'NONE',  ( 0.000000000000000000, -0.000000000000000000, 1.000000000000000000 ) ) ;
#5276 = ORIENTED_EDGE ( 'NONE', *, *, #7407, .T. ) ;
#5277 = CARTESIAN_POINT ( 'NONE',  ( -61.49999999999998579, 15.54166666666666607, 0.6339745962155628467 ) ) ;
#5278 = CARTESIAN_POINT ( 'NONE',  ( -61.13531646874997705, 9.911458332991934128, 1.000774730468978468 ) ) ;
#5279 = AXIS2_PLACEMENT_3D ( 'NONE', #8717, #8653, #8830 ) ;
#5280 = CARTESIAN_POINT ( 'NONE',  ( 0.000000000000000000, 0.000000000000000000, 0.000000000000000000 ) ) ;
#5281 = CARTESIAN_POINT ( 'NONE',  ( -61.13531646874998415, 15.57812499965860198, 1.500000000000002220 ) ) ;
#5282 = CARTESIAN_POINT ( 'NONE',  ( -60.99999999999998579, 13.48958333265053611, 0.9226497308103762673 ) ) ;
#5283 = CARTESIAN_POINT ( 'NONE',  ( 150.0000000000000000, -8.000000000000000000, 4.000000000000000000 ) ) ;
#5284 = ORIENTED_EDGE ( 'NONE', *, *, #2793, .T. ) ;
#5285 = CARTESIAN_POINT ( 'NONE',  ( -60.99999999999998579, 9.770833333333332149, 0.9226497308103762673 ) ) ;
#5286 = VECTOR ( 'NONE', #2959, 1000.000000000000000 ) ;
#5287 = AXIS2_PLACEMENT_3D ( 'NONE', #5352, #4470, #7817 ) ;
#5288 = CARTESIAN_POINT ( 'NONE',  ( -62.43234176562498305, 11.16145833299193590, 0.7511620957034662593 ) ) ;
#5289 = LINE ( 'NONE', #3409, #9909 ) ;
#5290 = DIRECTION ( 'NONE',  ( 0.000000000000000000, 0.000000000000000000, -1.000000000000000000 ) ) ;
#5291 = ORIENTED_EDGE ( 'NONE', *, *, #8473, .T. ) ;
#5292 = CARTESIAN_POINT ( 'NONE',  ( -60.99999999999998579, 11.22916666666666785, 2.077350269189628840 ) ) ;
#5293 = CARTESIAN_POINT ( 'NONE',  ( -62.99999999999998579, 10.12500000000000000, 1.500000000000001998 ) ) ;
#5294 = CIRCLE ( 'NONE', #10636, 1.000000000000000000 ) ;
#5295 = CARTESIAN_POINT ( 'NONE',  ( -61.99999999999998579, 14.32812499965860020, 2.498450539062049724 ) ) ;
#5296 = DIRECTION ( 'NONE',  ( 0.000000000000000000, 0.000000000000000000, -1.000000000000000000 ) ) ;
#5297 = CARTESIAN_POINT ( 'NONE',  ( -61.49999999999998579, 9.760416665983870033, 0.6339745962155628467 ) ) ;
#5298 = ORIENTED_EDGE ( 'NONE', *, *, #657, .F. ) ;
#5299 = EDGE_CURVE ( 'NONE', #8335, #7065, #2636, .T. ) ;
#5300 = DIRECTION ( 'NONE',  ( -0.000000000000000000, -0.000000000000000000, -1.000000000000000000 ) ) ;
#5301 = CARTESIAN_POINT ( 'NONE',  ( -62.99999999999998579, 13.37500000000000000, 1.500000000000001998 ) ) ;
#5302 = VECTOR ( 'NONE', #10735, 1000.000000000000000 ) ;
#5303 = CARTESIAN_POINT ( 'NONE',  ( -61.99999999999998579, 10.76562499965860020, 2.498450539062049724 ) ) ;
#5304 = AXIS2_PLACEMENT_3D ( 'NONE', #9404, #3512, #956 ) ;
#5305 = VERTEX_POINT ( 'NONE', #395 ) ;
#5306 = CARTESIAN_POINT ( 'NONE',  ( -61.56765823437498852, 10.34895833299193413, 2.248837904296538515 ) ) ;
#5307 = CARTESIAN_POINT ( 'NONE',  ( -77.99999999999998579, 11.49999999999999645, 5.000000000000000000 ) ) ;
#5308 = AXIS2_PLACEMENT_3D ( 'NONE', #5814, #4302, #36 ) ;
#5309 = CARTESIAN_POINT ( 'NONE',  ( -61.56765823437498142, 14.68229166632526805, 0.7511620957034663704 ) ) ;
#5310 = PLANE ( 'NONE',  #6957 ) ;
#5311 = VERTEX_POINT ( 'NONE', #8900 ) ;
#5312 = LINE ( 'NONE', #8834, #6026 ) ;
#5313 = ORIENTED_EDGE ( 'NONE', *, *, #9837, .F. ) ;
#5314 = CARTESIAN_POINT ( 'NONE',  ( -105.0000000000000000, 2.500000000000000000, 2.000000000000000000 ) ) ;
#5315 = CARTESIAN_POINT ( 'NONE',  ( -60.99999999999998579, 8.229166666666667851, 2.077350269189628840 ) ) ;
#5316 = LINE ( 'NONE', #10437, #6895 ) ;
#5317 = CARTESIAN_POINT ( 'NONE',  ( -120.0000000000000000, -15.00000000000001421, 5.000000000000004441 ) ) ;
#5318 = CARTESIAN_POINT ( 'NONE',  ( -61.13531646874997705, 14.66145833299193413, 1.000774730468978468 ) ) ;
#5319 = CARTESIAN_POINT ( 'NONE',  ( -62.43234176562498305, 9.161458332991935904, 0.7511620957034662593 ) ) ;
#5320 = EDGE_CURVE ( 'NONE', #6146, #6924, #6339, .T. ) ;
#5321 = CARTESIAN_POINT ( 'NONE',  ( -61.99999999999998579, 10.78124999931720218, 0.5000000000000013323 ) ) ;
#5322 = DIRECTION ( 'NONE',  ( -0.000000000000000000, -0.000000000000000000, -1.000000000000000000 ) ) ;
#5323 = CARTESIAN_POINT ( 'NONE',  ( -61.99999999999998579, 10.70312499965860198, 0.5015494609379544944 ) ) ;
#5324 = CARTESIAN_POINT ( 'NONE',  ( -77.99999999999998579, 11.49999999999999645, -2.000000000000001332 ) ) ;
#5325 = ORIENTED_EDGE ( 'NONE', *, *, #10878, .F. ) ;
#5326 = CARTESIAN_POINT ( 'NONE',  ( -62.99999999999998579, 14.39583333333333215, 2.077350269189627952 ) ) ;
#5327 = CARTESIAN_POINT ( 'NONE',  ( -61.73205080756886076, 13.02008544963257108, 0.5000000000000014433 ) ) ;
#5328 = DIRECTION ( 'NONE',  ( -1.000000000000000000, -0.000000000000000000, -0.000000000000000000 ) ) ;
#5329 = CARTESIAN_POINT ( 'NONE',  ( -61.56765823437498142, 12.61979166632526805, 0.7511620957034663704 ) ) ;
#5330 = CARTESIAN_POINT ( 'NONE',  ( -62.43234176562499016, 8.994791666325268054, 2.248837904296538071 ) ) ;
#5331 = PLANE ( 'NONE',  #9085 ) ;
#5332 =( BOUNDED_CURVE ( )  B_SPLINE_CURVE ( 2, ( #804, #8421, #7280, #9252, #5021, #3200, #6603, #5752, #9147 ),
 .UNSPECIFIED., .F., .T. ) 
 B_SPLINE_CURVE_WITH_KNOTS ( ( 3, 2, 2, 2, 3 ),
 ( 0.1796875000000000000, 0.1822916666666666574, 0.1875000000000000000, 0.1927083333333333426, 0.1953124999999999722 ),
 .UNSPECIFIED. ) 
 CURVE ( )  GEOMETRIC_REPRESENTATION_ITEM ( )  RATIONAL_B_SPLINE_CURVE ( ( 0.9330127018922194093, 0.9330127018922194093, 1.000000000000000000, 0.8660254037844387076, 1.000000000000000000, 0.8660254037844387076, 1.000000000000000000, 0.9330127018922200755, 0.9330127018922194093 ) ) 
 REPRESENTATION_ITEM ( '' )  );
#5333 = ORIENTED_EDGE ( 'NONE', *, *, #963, .F. ) ;
#5334 = LINE ( 'NONE', #6419, #139 ) ;
#5335 = AXIS2_PLACEMENT_3D ( 'NONE', #3752, #8041, #5638 ) ;
#5336 = CARTESIAN_POINT ( 'NONE',  ( -62.43234176562499016, 9.807291666325268054, 2.248837904296538071 ) ) ;
#5337 = DIRECTION ( 'NONE',  ( 0.000000000000000000, 0.000000000000000000, 1.000000000000000000 ) ) ;
#5338 = CARTESIAN_POINT ( 'NONE',  ( -62.86468353124999453, 14.70312499965860020, 1.500000000000002220 ) ) ;
#5339 = CARTESIAN_POINT ( 'NONE',  ( -62.99999999999998579, 14.84374999931720218, 1.500000000000001998 ) ) ;
#5340 = DIRECTION ( 'NONE',  ( 0.000000000000000000, 1.000000000000000000, 0.000000000000000000 ) ) ;
#5341 = ORIENTED_EDGE ( 'NONE', *, *, #10184, .T. ) ;
#5342 = ADVANCED_FACE ( 'NONE', ( #2897 ), #5433, .T. ) ;
#5343 = PRODUCT_DEFINITION ( 'UNKNOWN', '', #2150, #1298 ) ;
#5344 = CARTESIAN_POINT ( 'NONE',  ( -61.56765823437498852, 13.53645833299193413, 2.248837904296538515 ) ) ;
#5345 = CARTESIAN_POINT ( 'NONE',  ( -61.99999999999998579, 8.390624999658601979, 0.5015494609379544944 ) ) ;
#5346 = CARTESIAN_POINT ( 'NONE',  ( -62.49999999999998579, 8.333333333333333925, 0.6339745962155627357 ) ) ;
#5347 = ORIENTED_EDGE ( 'NONE', *, *, #9781, .T. ) ;
#5348 = CARTESIAN_POINT ( 'NONE',  ( -60.99999999999998579, 12.25000000000000000, 1.500000000000002220 ) ) ;
#5349 = CARTESIAN_POINT ( 'NONE',  ( -61.99999999999998579, 16.00000000000000000, 0.5000000000000041078 ) ) ;
#5350 = CARTESIAN_POINT ( 'NONE',  ( -61.13531646874998415, 14.36979166632527161, 1.999225269531026417 ) ) ;
#5351 = FILL_AREA_STYLE ('',( #1981 ) ) ;
#5352 = CARTESIAN_POINT ( 'NONE',  ( -105.0000000000000000, -2.500000000000000000, 4.000000000000000000 ) ) ;
#5353 = AXIS2_PLACEMENT_3D ( 'NONE', #2383, #10776, #7397 ) ;
#5354 = VECTOR ( 'NONE', #2663, 1000.000000000000000 ) ;
#5355 = CARTESIAN_POINT ( 'NONE',  ( -62.99999999999998579, 10.36458333265053433, 2.077350269189627952 ) ) ;
#5356 = VERTEX_POINT ( 'NONE', #2954 ) ;
#5357 = CARTESIAN_POINT ( 'NONE',  ( 140.0000000000000284, -8.000000000000000000, 3.000000000000000000 ) ) ;
#5358 = CARTESIAN_POINT ( 'NONE',  ( -61.49999999999998579, 10.01041666598387003, 0.6339745962155628467 ) ) ;
#5359 = AXIS2_PLACEMENT_3D ( 'NONE', #8309, #1914, #6022 ) ;
#5360 = CARTESIAN_POINT ( 'NONE',  ( -61.56765823437498142, 11.11979166632526805, 0.7511620957034663704 ) ) ;
#5361 = VECTOR ( 'NONE', #8154, 1000.000000000000000 ) ;
#5362 = PRESENTATION_STYLE_ASSIGNMENT (( #1152 ) ) ;
#5363 = ORIENTED_EDGE ( 'NONE', *, *, #5229, .T. ) ;
#5364 = CARTESIAN_POINT ( 'NONE',  ( -62.86468353124998742, 10.03645833299193235, 1.999225269531025972 ) ) ;
#5365 = DIRECTION ( 'NONE',  ( -1.000000000000000000, 1.110223024625156343E-15, 0.000000000000000000 ) ) ;
#5366 =( BOUNDED_CURVE ( )  B_SPLINE_CURVE ( 2, ( #10199, #5981, #8488, #872, #4253, #7658, #7715, #1768, #1156 ),
 .UNSPECIFIED., .F., .F. ) 
 B_SPLINE_CURVE_WITH_KNOTS ( ( 3, 2, 2, 2, 3 ),
 ( 0.7734375000000000000, 0.7760416666666666297, 0.7812500000000000000, 0.7864583333333333703, 0.7890625000000000000 ),
 .UNSPECIFIED. ) 
 CURVE ( )  GEOMETRIC_REPRESENTATION_ITEM ( )  RATIONAL_B_SPLINE_CURVE ( ( 0.9330127018922194093, 0.9330127018922194093, 1.000000000000000000, 0.8660254037844387076, 1.000000000000000000, 0.8660254037844387076, 1.000000000000000000, 0.9330127018922194093, 0.9330127018922194093 ) ) 
 REPRESENTATION_ITEM ( '' )  );
#5367 = AXIS2_PLACEMENT_3D ( 'NONE', #5401, #2084, #8977 ) ;
#5368 = CARTESIAN_POINT ( 'NONE',  ( -62.86468353124999453, 14.26562499965860020, 1.500000000000002220 ) ) ;
#5369 = CARTESIAN_POINT ( 'NONE',  ( 145.0000000000000284, -5.500000000000000000, 6.000000000000000000 ) ) ;
#5370 = VERTEX_POINT ( 'NONE', #1346 ) ;
#5371 = EDGE_CURVE ( 'NONE', #3072, #10303, #4353, .T. ) ;
#5372 = CARTESIAN_POINT ( 'NONE',  ( -60.99999999999998579, 10.47916666666666607, 2.077350269189628840 ) ) ;
#5373 = ORIENTED_EDGE ( 'NONE', *, *, #9615, .T. ) ;
#5374 = VECTOR ( 'NONE', #9002, 999.9999999999998863 ) ;
#5375 = DIRECTION ( 'NONE',  ( 0.000000000000000000, 1.000000000000000000, 0.000000000000000000 ) ) ;
#5376 = EDGE_CURVE ( 'NONE', #7235, #8381, #5379, .T. ) ;
#5377 = CARTESIAN_POINT ( 'NONE',  ( -62.43234176562499016, 15.99479166632526628, 2.248837904296538071 ) ) ;
#5378 = DIRECTION ( 'NONE',  ( 0.000000000000000000, 0.000000000000000000, -1.000000000000000000 ) ) ;
#5379 = LINE ( 'NONE', #511, #1398 ) ;
#5380 = CARTESIAN_POINT ( 'NONE',  ( 1.299999999999999156, 0.000000000000000000, 0.000000000000000000 ) ) ;
#5381 = CARTESIAN_POINT ( 'NONE',  ( -62.86468353124999453, 14.51562499965860020, 1.500000000000002220 ) ) ;
#5382 = CARTESIAN_POINT ( 'NONE',  ( -62.43234176562499016, 9.994791666325268054, 2.248837904296538071 ) ) ;
#5383 = UNCERTAINTY_MEASURE_WITH_UNIT (LENGTH_MEASURE( 1.000000000000000082E-05 ), #7766, 'distance_accuracy_value', 'NONE');
#5384 = LINE ( 'NONE', #1290, #2637 ) ;
#5385 = CARTESIAN_POINT ( 'NONE',  ( 146.0999999999999943, -5.500000000000000000, 6.000000000000000000 ) ) ;
#5386 = CARTESIAN_POINT ( 'NONE',  ( -61.99999999999998579, 10.95312499965860020, 0.5015494609379544944 ) ) ;
#5387 = CARTESIAN_POINT ( 'NONE',  ( -62.49999999999998579, 12.16666666666666607, 2.366025403784441483 ) ) ;
#5388 = VERTEX_POINT ( 'NONE', #6285 ) ;
#5389 = DIRECTION ( 'NONE',  ( -1.000000000000000000, 0.000000000000000000, -0.000000000000000000 ) ) ;
#5390 = CARTESIAN_POINT ( 'NONE',  ( -61.99999999999998579, 16.00000000000000000, 0.5000000000000041078 ) ) ;
#5391 = ORIENTED_EDGE ( 'NONE', *, *, #283, .F. ) ;
#5392 = CARTESIAN_POINT ( 'NONE',  ( -61.99999999999998579, 10.15624999931720041, 2.500000000000002665 ) ) ;
#5393 = CARTESIAN_POINT ( 'NONE',  ( -61.56765823437498142, 13.11979166632526805, 0.7511620957034663704 ) ) ;
#5394 = CARTESIAN_POINT ( 'NONE',  ( -62.86468353124998032, 9.432291666325268054, 1.000774730468978024 ) ) ;
#5395 = ORIENTED_EDGE ( 'NONE', *, *, #658, .T. ) ;
#5396 = CARTESIAN_POINT ( 'NONE',  ( -62.26794919243111082, 10.79241454900183328, 0.5000000000000013323 ) ) ;
#5397 = CARTESIAN_POINT ( 'NONE',  ( -61.56765823437498142, 9.682291666325268054, 0.7511620957034663704 ) ) ;
#5398 = DIRECTION ( 'NONE',  ( -5.551115123125782702E-17, 5.551115123125782702E-17, 1.000000000000000000 ) ) ;
#5399 = CARTESIAN_POINT ( 'NONE',  ( -61.13531646874998415, 15.34895833299193590, 1.000774730468978468 ) ) ;
#5400 = CARTESIAN_POINT ( 'NONE',  ( -62.99999999999998579, 15.07291666598386826, 0.9226497308103756012 ) ) ;
#5401 = CARTESIAN_POINT ( 'NONE',  ( 145.0000000000000284, -5.500000000000000000, 3.000000000000000888 ) ) ;
#5402 = VERTEX_POINT ( 'NONE', #10382 ) ;
#5403 = EDGE_CURVE ( 'NONE', #2273, #2258, #5316, .T. ) ;
#5404 = DIRECTION ( 'NONE',  ( 0.000000000000000000, 0.000000000000000000, -1.000000000000000000 ) ) ;
#5405 = ORIENTED_EDGE ( 'NONE', *, *, #9040, .F. ) ;
#5406 = ADVANCED_FACE ( 'NONE', ( #1226 ), #8728, .F. ) ;
#5407 = CARTESIAN_POINT ( 'NONE',  ( -62.86468353124999453, 12.95312499965860198, 1.500000000000002220 ) ) ;
#5408 = CARTESIAN_POINT ( 'NONE',  ( -61.99999999999998579, 16.00000000000000000, 1.500000000000002220 ) ) ;
#5409 = CARTESIAN_POINT ( 'NONE',  ( -62.99999999999998579, 10.61458333265053611, 2.077350269189627952 ) ) ;
#5410 = ORIENTED_EDGE ( 'NONE', *, *, #7451, .F. ) ;
#5411 = CARTESIAN_POINT ( 'NONE',  ( -61.99999999999998579, 12.31250000000000000, 0.3452994616207497591 ) ) ;
#5412 = LINE ( 'NONE', #5349, #414 ) ;
#5413 = CARTESIAN_POINT ( 'NONE',  ( -62.43234176562499016, 14.30729166632526983, 2.248837904296538071 ) ) ;
#5414 = CARTESIAN_POINT ( 'NONE',  ( -60.99999999999998579, 10.27083333333333393, 0.9226497308103762673 ) ) ;
#5415 = CARTESIAN_POINT ( 'NONE',  ( -61.49999999999998579, 11.01041666598386826, 0.6339745962155628467 ) ) ;
#5416 = ORIENTED_EDGE ( 'NONE', *, *, #6052, .T. ) ;
#5417 = CYLINDRICAL_SURFACE ( 'NONE', #10089, 0.9999999999999981126 ) ;
#5418 = DIRECTION ( 'NONE',  ( 0.000000000000000000, -1.000000000000000000, 0.000000000000000000 ) ) ;
#5419 = CARTESIAN_POINT ( 'NONE',  ( -62.86468353124998032, 12.43229166632526628, 1.000774730468978246 ) ) ;
#5420 = CARTESIAN_POINT ( 'NONE',  ( 0.000000000000000000, 0.2499999999999998335, -1.312875263449799101 ) ) ;
#5421 = ORIENTED_EDGE ( 'NONE', *, *, #9314, .T. ) ;
#5422 = EDGE_CURVE ( 'NONE', #7681, #9658, #7896, .T. ) ;
#5423 = CARTESIAN_POINT ( 'NONE',  ( -62.43234176562498305, 10.22395833299193413, 0.7511620957034662593 ) ) ;
#5424 = DIRECTION ( 'NONE',  ( -1.000000000000000000, -0.000000000000000000, -0.000000000000000000 ) ) ;
#5425 = CARTESIAN_POINT ( 'NONE',  ( -61.13531646874998415, 14.66145833299193590, 1.000774730468978468 ) ) ;
#5426 = FACE_OUTER_BOUND ( 'NONE', #9487, .T. ) ;
#5427 = VERTEX_POINT ( 'NONE', #2842 ) ;
#5428 = CYLINDRICAL_SURFACE ( 'NONE', #3031, 0.9999999999999981126 ) ;
#5429 = VERTEX_POINT ( 'NONE', #6228 ) ;
#5430 = CARTESIAN_POINT ( 'NONE',  ( -61.99999999999998579, 8.687500000000000000, 2.500000000000002665 ) ) ;
#5431 = CARTESIAN_POINT ( 'NONE',  ( -62.99999999999998579, 8.395833333333333925, 2.077350269189627952 ) ) ;
#5432 = CARTESIAN_POINT ( 'NONE',  ( -60.99999999999998579, 11.22916666666666607, 2.077350269189628840 ) ) ;
#5433 = PLANE ( 'NONE',  #3696 ) ;
#5434 = EDGE_CURVE ( 'NONE', #10100, #5639, #3303, .T. ) ;
#5435 = DIRECTION ( 'NONE',  ( -0.000000000000000000, -0.000000000000000000, -1.000000000000000000 ) ) ;
#5436 = CARTESIAN_POINT ( 'NONE',  ( -61.56765823437498142, 14.93229166632526805, 0.7511620957034663704 ) ) ;
#5437 = CARTESIAN_POINT ( 'NONE',  ( -61.13531646874998415, 10.07812499965860198, 1.500000000000002220 ) ) ;
#5438 = DIRECTION ( 'NONE',  ( -0.000000000000000000, -1.000000000000000000, -0.000000000000000000 ) ) ;
#5439 = LINE ( 'NONE', #9559, #9556 ) ;
#5440 = CARTESIAN_POINT ( 'NONE',  ( -62.86468353124998032, 10.99479166632526628, 1.000774730468978246 ) ) ;
#5441 = DIRECTION ( 'NONE',  ( -0.000000000000000000, -1.000000000000000000, -0.000000000000000000 ) ) ;
#5442 = VERTEX_POINT ( 'NONE', #10043 ) ;
#5443 = DIRECTION ( 'NONE',  ( -0.000000000000000000, -0.000000000000000000, -1.000000000000000000 ) ) ;
#5444 = ADVANCED_FACE ( 'NONE', ( #10728 ), #8233, .T. ) ;
#5445 = FACE_OUTER_BOUND ( 'NONE', #9968, .T. ) ;
#5446 = EDGE_LOOP ( 'NONE', ( #7439, #4671, #8814, #578 ) ) ;
#5447 = CARTESIAN_POINT ( 'NONE',  ( -62.86468353124999453, 12.70312499965860198, 1.500000000000002220 ) ) ;
#5448 = CARTESIAN_POINT ( 'NONE',  ( -61.56765823437498142, 9.619791666325268054, 0.7511620957034663704 ) ) ;
#5449 =( NAMED_UNIT ( * ) SI_UNIT ( $, .STERADIAN. ) SOLID_ANGLE_UNIT ( ) );
#5450 = ORIENTED_EDGE ( 'NONE', *, *, #1734, .T. ) ;
#5451 = CARTESIAN_POINT ( 'NONE',  ( -120.0000000000000000, -8.000000000000000000, 0.000000000000000000 ) ) ;
#5452 = CARTESIAN_POINT ( 'NONE',  ( -61.13531646874997705, 9.619791666325268054, 1.999225269531026417 ) ) ;
#5453 = COLOUR_RGB ( '',0.8941176470588234615, 0.8941176470588234615, 0.8941176470588234615 ) ;
#5454 = SHAPE_DEFINITION_REPRESENTATION ( #4034, #6156 ) ;
#5455 = CARTESIAN_POINT ( 'NONE',  ( -62.86468353124998032, 15.43229166632526805, 1.000774730468978246 ) ) ;
#5456 = CARTESIAN_POINT ( 'NONE',  ( -61.99999999999998579, 14.78124999931720218, 0.3452994616207497591 ) ) ;
#5457 = CARTESIAN_POINT ( 'NONE',  ( -61.49999999999998579, 14.67708333265053611, 2.366025403784441927 ) ) ;
#5458 = EDGE_LOOP ( 'NONE', ( #8088, #3690 ) ) ;
#5459 = PRESENTATION_STYLE_ASSIGNMENT (( #8868 ) ) ;
#5460 = ORIENTED_EDGE ( 'NONE', *, *, #9974, .T. ) ;
#5461 = AXIS2_PLACEMENT_3D ( 'NONE', #9283, #1617, #9330 ) ;
#5462 = CARTESIAN_POINT ( 'NONE',  ( -62.86468353124998032, 12.68229166632526628, 1.000774730468978024 ) ) ;
#5463 = CARTESIAN_POINT ( 'NONE',  ( -62.86468353124998032, 8.432291666325266277, 1.000774730468978246 ) ) ;
#5464 = VECTOR ( 'NONE', #7770, 1000.000000000000000 ) ;
#5465 = LINE ( 'NONE', #1424, #6799 ) ;
#5466 = VERTEX_POINT ( 'NONE', #4099 ) ;
#5467 = CARTESIAN_POINT ( 'NONE',  ( -60.99999999999998579, 13.00000000000000178, 1.500000000000002220 ) ) ;
#5468 = CARTESIAN_POINT ( 'NONE',  ( -61.56765823437498142, 13.68229166632526805, 0.7511620957034663704 ) ) ;
#5469 = CARTESIAN_POINT ( 'NONE',  ( -61.99999999999998579, 14.28124999931720218, 0.5000000000000013323 ) ) ;
#5470 = VECTOR ( 'NONE', #9328, 1000.000000000000000 ) ;
#5471 = CARTESIAN_POINT ( 'NONE',  ( -61.49999999999998579, 10.42708333265053611, 2.366025403784441927 ) ) ;
#5472 = EDGE_CURVE ( 'NONE', #1239, #10050, #7068, .T. ) ;
#5473 = ORIENTED_EDGE ( 'NONE', *, *, #8718, .F. ) ;
#5474 = VECTOR ( 'NONE', #1652, 1000.000000000000000 ) ;
#5475 = CARTESIAN_POINT ( 'NONE',  ( -49.99999999999998579, -15.00000000000001243, 0.000000000000000000 ) ) ;
#5476 = CARTESIAN_POINT ( 'NONE',  ( -61.56765823437498852, 12.78645833299193413, 2.248837904296538515 ) ) ;
#5477 = SURFACE_STYLE_FILL_AREA ( #441 ) ;
#5478 = VECTOR ( 'NONE', #3914, 1000.000000000000000 ) ;
#5479 = EDGE_LOOP ( 'NONE', ( #1596, #3767, #9870, #9991 ) ) ;
#5480 = PRESENTATION_LAYER_ASSIGNMENT (  '', '', ( #1232 ) ) ;
#5481 = CARTESIAN_POINT ( 'NONE',  ( -61.56765823437498142, 10.43229166632526983, 0.7511620957034663704 ) ) ;
#5482 = DIRECTION ( 'NONE',  ( -0.000000000000000000, 1.000000000000000000, -0.000000000000000000 ) ) ;
#5483 = TOROIDAL_SURFACE ( 'NONE', #6915, 1.336466033005844434, 0.5999999999999999778 ) ;
#5484 = CARTESIAN_POINT ( 'NONE',  ( -62.43234176562498305, 14.97395833299193590, 0.7511620957034662593 ) ) ;
#5485 = DIRECTION ( 'NONE',  ( -0.000000000000000000, -0.000000000000000000, -1.000000000000000000 ) ) ;
#5486 = ORIENTED_EDGE ( 'NONE', *, *, #10039, .T. ) ;
#5487 = LINE ( 'NONE', #7050, #7287 ) ;
#5488 = EDGE_CURVE ( 'NONE', #7998, #5865, #6712, .T. ) ;
#5489 = MECHANICAL_DESIGN_GEOMETRIC_PRESENTATION_REPRESENTATION (  '', ( #10823 ), #9580 ) ;
#5490 = ORIENTED_EDGE ( 'NONE', *, *, #1134, .F. ) ;
#5491 = UNCERTAINTY_MEASURE_WITH_UNIT (LENGTH_MEASURE( 1.000000000000000082E-05 ), #1967, 'distance_accuracy_value', 'NONE');
#5492 = CARTESIAN_POINT ( 'NONE',  ( -61.99999999999998579, 10.03124999931720218, 0.5000000000000013323 ) ) ;
#5493 = CARTESIAN_POINT ( 'NONE',  ( -62.99999999999998579, 8.125000000000000000, 1.500000000000001998 ) ) ;
#5494 = CIRCLE ( 'NONE', #7994, 1.000000000000000888 ) ;
#5495 = CARTESIAN_POINT ( 'NONE',  ( -61.73205080756886076, 11.30133545031536890, 0.5000000000000014433 ) ) ;
#5496 = CARTESIAN_POINT ( 'NONE',  ( 1.299999999999999156, 0.000000000000000000, 0.000000000000000000 ) ) ;
#5497 = CARTESIAN_POINT ( 'NONE',  ( -120.0000000000000000, -15.00000000000001421, 0.000000000000000000 ) ) ;
#5498 = CARTESIAN_POINT ( 'NONE',  ( -61.13531646874998415, 9.598958332991934128, 1.000774730468978468 ) ) ;
#5499 = PRODUCT_DEFINITION_FORMATION_WITH_SPECIFIED_SOURCE ( 'ANY', '', #7328, .NOT_KNOWN. ) ;
#5500 = DIRECTION ( 'NONE',  ( -0.000000000000000000, -1.000000000000000000, -0.000000000000000000 ) ) ;
#5501 = FACE_OUTER_BOUND ( 'NONE', #10256, .T. ) ;
#5502 = CARTESIAN_POINT ( 'NONE',  ( -62.43234176562499016, 10.55729166632526983, 2.248837904296538071 ) ) ;
#5503 = CARTESIAN_POINT ( 'NONE',  ( 0.000000000000000000, 0.000000000000000000, 4.000000000000000000 ) ) ;
#5504 = ORIENTED_EDGE ( 'NONE', *, *, #7580, .F. ) ;
#5505 = CARTESIAN_POINT ( 'NONE',  ( -60.99999999999998579, 13.94791666598387003, 2.077350269189628840 ) ) ;
#5506 = LINE ( 'NONE', #5390, #5018 ) ;
#5507 =( BOUNDED_CURVE ( )  B_SPLINE_CURVE ( 2, ( #3616, #4619, #9564, #7128, #10510, #5326, #2071, #8019, #3793 ),
 .UNSPECIFIED., .F., .T. ) 
 B_SPLINE_CURVE_WITH_KNOTS ( ( 3, 2, 2, 2, 3 ),
 ( 0.7890625000000000000, 0.7916666666666666297, 0.7968750000000000000, 0.8020833333333333703, 0.8046875000000000000 ),
 .UNSPECIFIED. ) 
 CURVE ( )  GEOMETRIC_REPRESENTATION_ITEM ( )  RATIONAL_B_SPLINE_CURVE ( ( 0.9330127018922194093, 0.9330127018922194093, 1.000000000000000000, 0.8660254037844387076, 1.000000000000000000, 0.8660254037844387076, 1.000000000000000000, 0.9330127018922194093, 0.9330127018922194093 ) ) 
 REPRESENTATION_ITEM ( '' )  );
#5508 = EDGE_LOOP ( 'NONE', ( #1362, #4006, #46, #8485 ) ) ;
#5509 = CARTESIAN_POINT ( 'NONE',  ( -61.49999999999998579, 10.17708333265053611, 2.366025403784441927 ) ) ;
#5510 = CARTESIAN_POINT ( 'NONE',  ( -62.86468353124998032, 12.68229166632526983, 1.000774730468978246 ) ) ;
#5511 = B_SPLINE_CURVE_WITH_KNOTS ( 'NONE', 3,
 ( #9657, #1271, #3049, #8773, #9596, #3703 ),
 .UNSPECIFIED., .F., .F.,
 ( 4, 2, 4 ),
 ( 0.0005861251363949650413, 0.001008091297609326094, 0.001430057458823687363 ),
 .UNSPECIFIED. ) ;
#5512 = CARTESIAN_POINT ( 'NONE',  ( -61.13531646874997705, 9.557291666325269830, 1.999225269531026417 ) ) ;
#5513 = SURFACE_STYLE_USAGE ( .BOTH. , #7243 ) ;
#5514 = ORIENTED_EDGE ( 'NONE', *, *, #8885, .F. ) ;
#5515 = CARTESIAN_POINT ( 'NONE',  ( -62.99999999999998579, 15.85416666666666430, 0.9226497308103756012 ) ) ;
#5516 = CARTESIAN_POINT ( 'NONE',  ( -62.43234176562498305, 11.47395833299193590, 0.7511620957034662593 ) ) ;
#5517 = CARTESIAN_POINT ( 'NONE',  ( -62.43234176562499016, 15.24479166632526805, 2.248837904296538071 ) ) ;
#5518 = CARTESIAN_POINT ( 'NONE',  ( -62.49999999999998579, 14.63541666598387003, 2.366025403784441483 ) ) ;
#5519 = DIRECTION ( 'NONE',  ( 1.000000000000000000, 0.000000000000000000, 0.000000000000000000 ) ) ;
#5520 = VERTEX_POINT ( 'NONE', #9003 ) ;
#5521 = CARTESIAN_POINT ( 'NONE',  ( -61.99999999999998579, 16.03124999931720041, 0.5000000000000013323 ) ) ;
#5522 = VERTEX_POINT ( 'NONE', #2331 ) ;
#5523 = CARTESIAN_POINT ( 'NONE',  ( -61.13531646874997705, 12.80729166632526983, 1.999225269531026417 ) ) ;
#5524 = CARTESIAN_POINT ( 'NONE',  ( -62.43234176562498305, 8.411458332991934128, 0.7511620957034662593 ) ) ;
#5525 = CARTESIAN_POINT ( 'NONE',  ( -62.99999999999998579, 10.57291666598387181, 0.9226497308103756012 ) ) ;
#5526 = VERTEX_POINT ( 'NONE', #3945 ) ;
#5527 = CARTESIAN_POINT ( 'NONE',  ( -61.99999999999998579, 12.06250000000000000, 0.3452994616207497591 ) ) ;
#5528 = EDGE_CURVE ( 'NONE', #2070, #1239, #6618, .T. ) ;
#5529 = EDGE_CURVE ( 'NONE', #3964, #40, #2379, .T. ) ;
#5530 = CARTESIAN_POINT ( 'NONE',  ( -62.26794919243111082, 13.29241454900183328, 0.5000000000000013323 ) ) ;
#5531 = DIRECTION ( 'NONE',  ( -0.000000000000000000, -0.000000000000000000, -1.000000000000000000 ) ) ;
#5532 = CARTESIAN_POINT ( 'NONE',  ( -61.99999999999998579, 10.78124999931720396, 0.3452994616207497591 ) ) ;
#5533 = ORIENTED_EDGE ( 'NONE', *, *, #1100, .F. ) ;
#5534 = AXIS2_PLACEMENT_3D ( 'NONE', #5789, #5950, #8675 ) ;
#5535 = CARTESIAN_POINT ( 'NONE',  ( -62.49999999999998579, 13.41666666666666785, 2.366025403784441483 ) ) ;
#5536 = CARTESIAN_POINT ( 'NONE',  ( -61.56765823437498142, 12.36979166632526805, 0.7511620957034663704 ) ) ;
#5537 = DIRECTION ( 'NONE',  ( -1.000000000000000000, -0.000000000000000000, -0.000000000000000000 ) ) ;
#5538 = ORIENTED_EDGE ( 'NONE', *, *, #4533, .F. ) ;
#5539 = VECTOR ( 'NONE', #6221, 1000.000000000000000 ) ;
#5540 = AXIS2_PLACEMENT_3D ( 'NONE', #10705, #9872, #2260 ) ;
#5541 = CARTESIAN_POINT ( 'NONE',  ( -61.13531646874998415, 10.89062499965860020, 1.500000000000002220 ) ) ;
#5542 = DIRECTION ( 'NONE',  ( 0.000000000000000000, 0.000000000000000000, 1.000000000000000000 ) ) ;
#5543 = CARTESIAN_POINT ( 'NONE',  ( -62.86468353124998742, 16.03645833299193768, 1.999225269531025972 ) ) ;
#5544 = CARTESIAN_POINT ( 'NONE',  ( -61.99999999999998579, 15.81250000000000000, 0.5000000000000013323 ) ) ;
#5545 = ORIENTED_EDGE ( 'NONE', *, *, #4892, .F. ) ;
#5546 = VECTOR ( 'NONE', #10115, 1000.000000000000000 ) ;
#5547 = DIRECTION ( 'NONE',  ( 0.000000000000000000, 0.000000000000000000, -1.000000000000000000 ) ) ;
#5548 = ADVANCED_FACE ( 'NONE', ( #10772 ), #9842, .T. ) ;
#5549 = AXIS2_PLACEMENT_3D ( 'NONE', #6318, #1080, #6085 ) ;
#5550 = ADVANCED_FACE ( 'NONE', ( #3998 ), #8278, .T. ) ;
#5551 = ORIENTED_EDGE ( 'NONE', *, *, #3464, .F. ) ;
#5552 = CARTESIAN_POINT ( 'NONE',  ( 145.0000000000000284, 5.500000000000000000, 0.000000000000000000 ) ) ;
#5553 = CARTESIAN_POINT ( 'NONE',  ( -62.49999999999998579, 9.333333333333333925, 0.6339745962155627357 ) ) ;
#5554 = CARTESIAN_POINT ( 'NONE',  ( -61.49999999999998579, 11.20833333333333393, 2.366025403784441927 ) ) ;
#5555 = APPLICATION_CONTEXT ( 'automotive_design' ) ;
#5556 = CARTESIAN_POINT ( 'NONE',  ( -61.99999999999998579, 12.06250000000000000, 0.5000000000000013323 ) ) ;
#5557 = DIRECTION ( 'NONE',  ( 0.000000000000000000, 0.000000000000000000, -1.000000000000000000 ) ) ;
#5558 = AXIS2_PLACEMENT_3D ( 'NONE', #2030, #2250, #9636 ) ;
#5559 = ADVANCED_FACE ( 'NONE', ( #718 ), #10880, .T. ) ;
#5560 = CARTESIAN_POINT ( 'NONE',  ( -62.86468353124998742, 10.47395833299193413, 1.999225269531025972 ) ) ;
#5561 = FACE_OUTER_BOUND ( 'NONE', #2577, .T. ) ;
#5562 = CARTESIAN_POINT ( 'NONE',  ( -61.13531646874998415, 11.64062499965860198, 1.500000000000002220 ) ) ;
#5563 = CARTESIAN_POINT ( 'NONE',  ( -61.99999999999998579, 12.18749999999999822, 2.500000000000002665 ) ) ;
#5564 = ORIENTED_EDGE ( 'NONE', *, *, #4258, .F. ) ;
#5565 = LINE ( 'NONE', #8963, #9769 ) ;
#5566 = DIRECTION ( 'NONE',  ( -1.000000000000000000, 0.000000000000000000, 0.000000000000000000 ) ) ;
#5567 = AXIS2_PLACEMENT_3D ( 'NONE', #6284, #5378, #1165 ) ;
#5568 = ORIENTED_EDGE ( 'NONE', *, *, #5488, .T. ) ;
#5569 = CARTESIAN_POINT ( 'NONE',  ( -61.99999999999998579, 15.68749999999999645, 2.500000000000002665 ) ) ;
#5570 = CARTESIAN_POINT ( 'NONE',  ( -62.86468353124999453, 13.20312499965860198, 1.500000000000002220 ) ) ;
#5571 = CARTESIAN_POINT ( 'NONE',  ( -62.86468353124999453, 10.22395833299193413, 1.999225269531025750 ) ) ;
#5572 = CARTESIAN_POINT ( 'NONE',  ( -62.26794919243111082, 8.676335450315370679, 2.500000000000003109 ) ) ;
#5573 = ORIENTED_EDGE ( 'NONE', *, *, #741, .T. ) ;
#5574 = CARTESIAN_POINT ( 'NONE',  ( -61.99999999999998579, 16.00000000000000000, 4.000000000000004441 ) ) ;
#5575 = CARTESIAN_POINT ( 'NONE',  ( -62.43234176562499016, 11.80729166632526805, 2.248837904296538071 ) ) ;
#5576 = EDGE_CURVE ( 'NONE', #9306, #5247, #9546, .T. ) ;
#5577 = CARTESIAN_POINT ( 'NONE',  ( -37.99999999999999289, -14.00000000000000888, 5.000000000000000000 ) ) ;
#5578 = CARTESIAN_POINT ( 'NONE',  ( -62.99999999999998579, 15.86458333265053788, 2.077350269189627952 ) ) ;
#5579 = LINE ( 'NONE', #2975, #10339 ) ;
#5580 = VERTEX_POINT ( 'NONE', #10670 ) ;
#5581 = FACE_BOUND ( 'NONE', #10814, .T. ) ;
#5582 = ORIENTED_EDGE ( 'NONE', *, *, #6990, .T. ) ;
#5583 =( BOUNDED_CURVE ( )  B_SPLINE_CURVE ( 2, ( #9004, #7339, #9997, #8328, #7447, #1347, #9787, #2332, #10828 ),
 .UNSPECIFIED., .F., .F. ) 
 B_SPLINE_CURVE_WITH_KNOTS ( ( 3, 2, 2, 2, 3 ),
 ( 0.02343749999999996531, 0.02604166666666666782, 0.03125000000000000000, 0.03645833333333333565, 0.03906250000000002082 ),
 .UNSPECIFIED. ) 
 CURVE ( )  GEOMETRIC_REPRESENTATION_ITEM ( )  RATIONAL_B_SPLINE_CURVE ( ( 0.9330127018922194093, 0.9330127018922185211, 1.000000000000000000, 0.8660254037844387076, 1.000000000000000000, 0.8660254037844387076, 1.000000000000000000, 0.9330127018922187432, 0.9330127018922192983 ) ) 
 REPRESENTATION_ITEM ( '' )  );
#5584 = ADVANCED_FACE ( 'NONE', ( #1446 ), #2891, .T. ) ;
#5585 = CARTESIAN_POINT ( 'NONE',  ( -62.86468353124999453, 12.22395833299193413, 1.999225269531025750 ) ) ;
#5586 = CARTESIAN_POINT ( 'NONE',  ( -61.13531646874998415, 9.307291666325268054, 1.999225269531026417 ) ) ;
#5587 = DIRECTION ( 'NONE',  ( -0.000000000000000000, -1.000000000000000000, -0.000000000000000000 ) ) ;
#5588 = ORIENTED_EDGE ( 'NONE', *, *, #6394, .T. ) ;
#5589 = CARTESIAN_POINT ( 'NONE',  ( -61.99999999999998579, 12.81250000000000000, 0.3452994616207497591 ) ) ;
#5590 = CARTESIAN_POINT ( 'NONE',  ( -61.73205080756885366, 8.948664549684629321, 2.500000000000001332 ) ) ;
#5591 = EDGE_CURVE ( 'NONE', #4539, #1599, #1469, .T. ) ;
#5592 = CARTESIAN_POINT ( 'NONE',  ( -62.99999999999998579, 10.82291666598387003, 0.9226497308103756012 ) ) ;
#5593 = DIRECTION ( 'NONE',  ( 0.000000000000000000, 0.000000000000000000, 1.000000000000000000 ) ) ;
#5594 = ADVANCED_FACE ( 'NONE', ( #3182 ), #1518, .T. ) ;
#5595 = CARTESIAN_POINT ( 'NONE',  ( -61.99999999999998579, 13.26562499965860198, 2.498450539062049724 ) ) ;
#5596 = CARTESIAN_POINT ( 'NONE',  ( -60.99999999999998579, 15.97916666666666607, 2.077350269189628840 ) ) ;
#5597 = ORIENTED_EDGE ( 'NONE', *, *, #10656, .T. ) ;
#5598 = CARTESIAN_POINT ( 'NONE',  ( -61.56765823437498142, 11.18229166632526805, 0.7511620957034663704 ) ) ;
#5599 = DIRECTION ( 'NONE',  ( -0.000000000000000000, -1.000000000000000000, -0.000000000000000000 ) ) ;
#5600 = CARTESIAN_POINT ( 'NONE',  ( -62.86468353124999453, 15.76562499965860198, 1.500000000000002220 ) ) ;
#5601 = ORIENTED_EDGE ( 'NONE', *, *, #2763, .T. ) ;
#5602 = DIRECTION ( 'NONE',  ( 0.000000000000000000, -1.000000000000000000, 0.000000000000000000 ) ) ;
#5603 = ORIENTED_EDGE ( 'NONE', *, *, #811, .T. ) ;
#5604 = PRODUCT_DEFINITION_CONTEXT ( 'detailed design', #4853, 'design' ) ;
#5605 = CYLINDRICAL_SURFACE ( 'NONE', #3387, 0.9999999999999981126 ) ;
#5606 = CARTESIAN_POINT ( 'NONE',  ( -61.99999999999998579, 9.437500000000000000, 2.654700538379254571 ) ) ;
#5607 = FACE_OUTER_BOUND ( 'NONE', #9470, .T. ) ;
#5608 = CARTESIAN_POINT ( 'NONE',  ( -61.99999999999998579, 15.03124999931720218, 0.5000000000000013323 ) ) ;
#5609 = DIRECTION ( 'NONE',  ( 0.000000000000000000, 0.000000000000000000, -1.000000000000000000 ) ) ;
#5610 = EDGE_CURVE ( 'NONE', #5765, #8110, #4951, .T. ) ;
#5611 = CARTESIAN_POINT ( 'NONE',  ( -120.0000000000000000, -8.000000000000000000, 3.000000000000000000 ) ) ;
#5612 = CARTESIAN_POINT ( 'NONE',  ( -62.86468353124998032, 11.99479166632526805, 1.000774730468978246 ) ) ;
#5613 = EDGE_CURVE ( 'NONE', #1330, #3363, #4799, .T. ) ;
#5614 = PLANE ( 'NONE',  #5353 ) ;
#5615 = ORIENTED_EDGE ( 'NONE', *, *, #5084, .T. ) ;
#5616 = CARTESIAN_POINT ( 'NONE',  ( -61.73205080756885366, 9.167414549001831503, 2.500000000000001332 ) ) ;
#5617 = CARTESIAN_POINT ( 'NONE',  ( -61.49999999999998579, 15.29166666666666607, 0.6339745962155628467 ) ) ;
#5618 = VERTEX_POINT ( 'NONE', #10014 ) ;
#5619 = CARTESIAN_POINT ( 'NONE',  ( -61.73205080756886076, 13.66741454900183150, 2.500000000000003109 ) ) ;
#5620 = CARTESIAN_POINT ( 'NONE',  ( -62.86468353124998742, 14.22395833299193590, 1.999225269531025972 ) ) ;
#5621 = CARTESIAN_POINT ( 'NONE',  ( -61.56765823437498142, 10.36979166632526983, 0.7511620957034663704 ) ) ;
#5622 = CARTESIAN_POINT ( 'NONE',  ( -62.49999999999998579, 8.166666666666667851, 2.366025403784441483 ) ) ;
#5623 = ORIENTED_EDGE ( 'NONE', *, *, #388, .T. ) ;
#5624 = LINE ( 'NONE', #4789, #3324 ) ;
#5625 = CARTESIAN_POINT ( 'NONE',  ( -61.13531646874997705, 11.11979166632526805, 1.999225269531026417 ) ) ;
#5626 = APPLICATION_PROTOCOL_DEFINITION ( 'draft international standard', 'automotive_design', 1998, #6209 ) ;
#5627 = CARTESIAN_POINT ( 'NONE',  ( -62.86468353124998742, 15.97395833299193590, 1.999225269531025972 ) ) ;
#5628 = CARTESIAN_POINT ( 'NONE',  ( -61.49999999999998579, 15.42708333265053611, 2.366025403784441927 ) ) ;
#5629 = CARTESIAN_POINT ( 'NONE',  ( -57.99999999999998579, -14.00000000000001243, -0.1418111474832477736 ) ) ;
#5630 = ORIENTED_EDGE ( 'NONE', *, *, #57, .T. ) ;
#5631 = DIRECTION ( 'NONE',  ( -0.000000000000000000, -1.000000000000000000, -0.000000000000000000 ) ) ;
#5632 = CARTESIAN_POINT ( 'NONE',  ( 0.5000000000000000000, 0.000000000000000000, 0.000000000000000000 ) ) ;
#5633 = ORIENTED_EDGE ( 'NONE', *, *, #1384, .F. ) ;
#5634 = ADVANCED_FACE ( 'NONE', ( #9181 ), #8144, .T. ) ;
#5635 = CARTESIAN_POINT ( 'NONE',  ( -61.13531646874997705, 13.55729166632526805, 1.999225269531026417 ) ) ;
#5636 = CARTESIAN_POINT ( 'NONE',  ( -62.86468353124998742, 9.973958332991932352, 1.999225269531025972 ) ) ;
#5637 = PRESENTATION_LAYER_ASSIGNMENT (  '', '', ( #1908 ) ) ;
#5638 = DIRECTION ( 'NONE',  ( -1.000000000000000000, 0.000000000000000000, 0.000000000000000000 ) ) ;
#5639 = VERTEX_POINT ( 'NONE', #6422 ) ;
#5640 = CARTESIAN_POINT ( 'NONE',  ( -61.49999999999998579, 14.20833333333333393, 2.366025403784441927 ) ) ;
#5641 = PRODUCT_DEFINITION_SHAPE ( 'NONE', 'NONE',  #10990 ) ;
#5642 = DIRECTION ( 'NONE',  ( -0.000000000000000000, -0.000000000000000000, -1.000000000000000000 ) ) ;
#5643 = CARTESIAN_POINT ( 'NONE',  ( -60.99999999999998579, 12.21874999931720218, 1.500000000000002220 ) ) ;
#5644 =( BOUNDED_CURVE ( )  B_SPLINE_CURVE ( 2, ( #6793, #10059, #2449, #10213, #6736, #5841, #8451, #1784, #10943 ),
 .UNSPECIFIED., .F., .T. ) 
 B_SPLINE_CURVE_WITH_KNOTS ( ( 3, 2, 2, 2, 3 ),
 ( 0.6484375000000000000, 0.6510416666666666297, 0.6562500000000000000, 0.6614583333333333703, 0.6640625000000000000 ),
 .UNSPECIFIED. ) 
 CURVE ( )  GEOMETRIC_REPRESENTATION_ITEM ( )  RATIONAL_B_SPLINE_CURVE ( ( 0.9330127018922194093, 0.9330127018922194093, 1.000000000000000000, 0.8660254037844387076, 1.000000000000000000, 0.8660254037844387076, 1.000000000000000000, 0.9330127018922194093, 0.9330127018922194093 ) ) 
 REPRESENTATION_ITEM ( '' )  );
#5645 = AXIS2_PLACEMENT_3D ( 'NONE', #6732, #3491, #4318 ) ;
#5646 = CARTESIAN_POINT ( 'NONE',  ( 0.5000000000000000000, -0.2500000000000001665, 1.911797424705720116 ) ) ;
#5647 = CARTESIAN_POINT ( 'NONE',  ( -62.86468353124998742, 13.22395833299193235, 1.999225269531025972 ) ) ;
#5648 = DIRECTION ( 'NONE',  ( -0.000000000000000000, 0.000000000000000000, 1.000000000000000000 ) ) ;
#5649 = ORIENTED_EDGE ( 'NONE', *, *, #5787, .T. ) ;
#5650 = CARTESIAN_POINT ( 'NONE',  ( -62.43234176562499016, 11.05729166632526805, 2.248837904296538071 ) ) ;
#5651 = EDGE_CURVE ( 'NONE', #7681, #4004, #7410, .T. ) ;
#5652 = AXIS2_PLACEMENT_3D ( 'NONE', #2005, #7898, #276 ) ;
#5653 = CARTESIAN_POINT ( 'NONE',  ( -62.43234176562498305, 15.97395833299193590, 0.7511620957034662593 ) ) ;
#5654 = ORIENTED_EDGE ( 'NONE', *, *, #3655, .F. ) ;
#5655 = DIRECTION ( 'NONE',  ( 0.000000000000000000, 0.000000000000000000, -1.000000000000000000 ) ) ;
#5656 = AXIS2_PLACEMENT_3D ( 'NONE', #9804, #7359, #10846 ) ;
#5657 = AXIS2_PLACEMENT_3D ( 'NONE', #7487, #6032, #5075 ) ;
#5658 = ORIENTED_EDGE ( 'NONE', *, *, #8113, .T. ) ;
#5659 = CARTESIAN_POINT ( 'NONE',  ( -61.99999999999997868, 8.781249999317202182, 0.5000000000000013323 ) ) ;
#5660 = CARTESIAN_POINT ( 'NONE',  ( -62.49999999999998579, 10.16666666666666785, 2.366025403784441483 ) ) ;
#5661 = CARTESIAN_POINT ( 'NONE',  ( -61.99999999999998579, 11.93750000000000000, 2.500000000000002665 ) ) ;
#5662 = DIRECTION ( 'NONE',  ( -0.000000000000000000, -1.000000000000000000, -0.000000000000000000 ) ) ;
#5663 = CARTESIAN_POINT ( 'NONE',  ( -62.26794919243111082, 14.79241454900183150, 0.5000000000000013323 ) ) ;
#5664 = EDGE_CURVE ( 'NONE', #9779, #4602, #6587, .T. ) ;
#5665 = VECTOR ( 'NONE', #5300, 1000.000000000000000 ) ;
#5666 = DIRECTION ( 'NONE',  ( -1.000000000000000000, -0.000000000000000000, -0.000000000000000000 ) ) ;
#5667 = CARTESIAN_POINT ( 'NONE',  ( -61.99999999999998579, 11.95312499965860198, 0.5015494609379544944 ) ) ;
#5668 = MECHANICAL_DESIGN_GEOMETRIC_PRESENTATION_REPRESENTATION (  '', ( #9935 ), #5839 ) ;
#5669 = CARTESIAN_POINT ( 'NONE',  ( -62.26794919243111082, 14.64508544963257464, 2.500000000000003109 ) ) ;
#5670 = ORIENTED_EDGE ( 'NONE', *, *, #10147, .T. ) ;
#5671 = LINE ( 'NONE', #2235, #5125 ) ;
#5672 = CARTESIAN_POINT ( 'NONE',  ( -120.0000000000000000, -15.00000000000001421, 3.000000000000002665 ) ) ;
#5673 = CIRCLE ( 'NONE', #8339, 6.000000000000005329 ) ;
#5674 = ORIENTED_EDGE ( 'NONE', *, *, #3929, .T. ) ;
#5675 = DIRECTION ( 'NONE',  ( 0.000000000000000000, 0.000000000000000000, -1.000000000000000000 ) ) ;
#5676 = CARTESIAN_POINT ( 'NONE',  ( -62.86468353124998032, 14.43229166632526805, 1.000774730468978246 ) ) ;
#5677 = ADVANCED_FACE ( 'NONE', ( #2347 ), #3969, .F. ) ;
#5678 = CARTESIAN_POINT ( 'NONE',  ( -61.99999999999999289, 9.640624999658601979, 0.5015494609379544944 ) ) ;
#5679 =( GEOMETRIC_REPRESENTATION_CONTEXT ( 3 ) GLOBAL_UNCERTAINTY_ASSIGNED_CONTEXT ( ( #6600 ) ) GLOBAL_UNIT_ASSIGNED_CONTEXT ( ( #10706, #10646, #1201 ) ) REPRESENTATION_CONTEXT ( 'NONE', 'WORKASPACE' ) );
#5680 = CARTESIAN_POINT ( 'NONE',  ( -61.73205080756886076, 14.55133545031536890, 0.5000000000000014433 ) ) ;
#5681 = CARTESIAN_POINT ( 'NONE',  ( -51.99999999999999289, 3.184081677783117796E-15, 10.99999999999999289 ) ) ;
#5682 = CARTESIAN_POINT ( 'NONE',  ( -61.56765823437498852, 11.84895833299193413, 2.248837904296538515 ) ) ;
#5683 = CARTESIAN_POINT ( 'NONE',  ( -61.99999999999998579, 15.70312499965860198, 0.5015494609379544944 ) ) ;
#5684 = CONTEXT_DEPENDENT_SHAPE_REPRESENTATION ( #2652, #4298 ) ;
#5685 = DIRECTION ( 'NONE',  ( -1.000000000000000000, -0.000000000000000000, -0.000000000000000000 ) ) ;
#5686 = CARTESIAN_POINT ( 'NONE',  ( -61.49999999999998579, 15.92708333265053433, 2.366025403784441927 ) ) ;
#5687 = CARTESIAN_POINT ( 'NONE',  ( -62.26794919243111082, 10.32366454968463287, 0.4999999999999982792 ) ) ;
#5688 = VERTEX_POINT ( 'NONE', #1566 ) ;
#5689 = LINE ( 'NONE', #2454, #9044 ) ;
#5690 = DIRECTION ( 'NONE',  ( -0.000000000000000000, -0.000000000000000000, -1.000000000000000000 ) ) ;
#5691 = CARTESIAN_POINT ( 'NONE',  ( -61.56765823437498142, 14.61979166632526805, 0.7511620957034663704 ) ) ;
#5692 = CARTESIAN_POINT ( 'NONE',  ( -61.13531646874998415, 10.07812499965860198, 1.500000000000002220 ) ) ;
#5693 = PLANE ( 'NONE',  #7865 ) ;
#5694 = EDGE_LOOP ( 'NONE', ( #10, #9413, #7170, #5973, #1932, #8095, #6662, #7528 ) ) ;
#5695 = CARTESIAN_POINT ( 'NONE',  ( -60.99999999999998579, 13.50000000000000000, 1.500000000000002220 ) ) ;
#5696 = CARTESIAN_POINT ( 'NONE',  ( -61.49999999999998579, 9.041666666666666075, 0.6339745962155628467 ) ) ;
#5697 = EDGE_CURVE ( 'NONE', #10833, #9209, #4497, .T. ) ;
#5698 = CARTESIAN_POINT ( 'NONE',  ( -62.99999999999998579, 12.36458333265053611, 2.077350269189627952 ) ) ;
#5699 = CARTESIAN_POINT ( 'NONE',  ( -62.86468353124999453, 14.20312499965860020, 1.500000000000002220 ) ) ;
#5700 = ORIENTED_EDGE ( 'NONE', *, *, #339, .T. ) ;
#5701 = CARTESIAN_POINT ( 'NONE',  ( -61.13531646874998415, 11.14062499965860020, 1.500000000000002220 ) ) ;
#5702 =( BOUNDED_CURVE ( )  B_SPLINE_CURVE ( 2, ( #7724, #881, #5939, #51, #5205, #3435, #935, #10204, #2552 ),
 .UNSPECIFIED., .F., .T. ) 
 B_SPLINE_CURVE_WITH_KNOTS ( ( 3, 2, 2, 2, 3 ),
 ( 0.4140625000000000000, 0.4166666666666666852, 0.4218750000000000000, 0.4270833333333333148, 0.4296875000000000555 ),
 .UNSPECIFIED. ) 
 CURVE ( )  GEOMETRIC_REPRESENTATION_ITEM ( )  RATIONAL_B_SPLINE_CURVE ( ( 0.9330127018922194093, 0.9330127018922194093, 1.000000000000000000, 0.8660254037844387076, 1.000000000000000000, 0.8660254037844387076, 1.000000000000000000, 0.9330127018922178550, 0.9330127018922192983 ) ) 
 REPRESENTATION_ITEM ( '' )  );
#5703 = CARTESIAN_POINT ( 'NONE',  ( -61.99999999999998579, 12.15624999931720041, 2.500000000000002665 ) ) ;
#5704 = CIRCLE ( 'NONE', #6972, 2.500000000000002220 ) ;
#5705 = CARTESIAN_POINT ( 'NONE',  ( -61.56765823437498852, 16.09895833299193768, 2.248837904296538515 ) ) ;
#5706 = ORIENTED_EDGE ( 'NONE', *, *, #6586, .F. ) ;
#5707 = DIRECTION ( 'NONE',  ( -1.000000000000000000, 0.000000000000000000, 0.000000000000000000 ) ) ;
#5708 = CONICAL_SURFACE ( 'NONE', #6255, 6.000000000000005329, 0.7853981633974479459 ) ;
#5709 = VERTEX_POINT ( 'NONE', #7305 ) ;
#5710 = FACE_OUTER_BOUND ( 'NONE', #1693, .T. ) ;
#5711 = CARTESIAN_POINT ( 'NONE',  ( -62.49999999999998579, 9.916666666666667851, 2.366025403784441483 ) ) ;
#5712 = CARTESIAN_POINT ( 'NONE',  ( -105.0000000000000000, -2.500000000000000000, 2.000000000000000000 ) ) ;
#5713 = CARTESIAN_POINT ( 'NONE',  ( -61.99999999999998579, 8.203124999658601979, 0.5015494609379544944 ) ) ;
#5714 = DIRECTION ( 'NONE',  ( -1.000000000000000000, 0.000000000000000000, 0.000000000000000000 ) ) ;
#5715 = ADVANCED_FACE ( 'NONE', ( #2199 ), #2458, .T. ) ;
#5716 = CARTESIAN_POINT ( 'NONE',  ( -61.99999999999998579, 15.53124999931720041, 0.5000000000000013323 ) ) ;
#5717 = AXIS2_PLACEMENT_3D ( 'NONE', #6333, #2945, #2889 ) ;
#5718 = VECTOR ( 'NONE', #3778, 1000.000000000000000 ) ;
#5719 = CARTESIAN_POINT ( 'NONE',  ( -61.13531646874998415, 12.36979166632526628, 1.999225269531026417 ) ) ;
#5720 = DIRECTION ( 'NONE',  ( -0.000000000000000000, -0.000000000000000000, -1.000000000000000000 ) ) ;
#5721 = EDGE_LOOP ( 'NONE', ( #2990, #3203, #803, #2984 ) ) ;
#5722 = CARTESIAN_POINT ( 'NONE',  ( -61.99999999999998579, 9.062500000000000000, 0.5000000000000013323 ) ) ;
#5723 = PRODUCT_DEFINITION_SHAPE ( 'NONE', 'NONE',  #6528 ) ;
#5724 = ADVANCED_FACE ( 'NONE', ( #10691 ), #3081, .T. ) ;
#5725 = EDGE_CURVE ( 'NONE', #7283, #5113, #4268, .T. ) ;
#5726 = PLANE ( 'NONE',  #914 ) ;
#5727 = MECHANICAL_DESIGN_GEOMETRIC_PRESENTATION_REPRESENTATION (  '', ( #7331 ), #8386 ) ;
#5728 = CARTESIAN_POINT ( 'NONE',  ( -104.9999999999999289, -15.00000000000001421, 83.15773105863907233 ) ) ;
#5729 = CARTESIAN_POINT ( 'NONE',  ( -61.13531646874998415, 14.32812499965860020, 1.500000000000002220 ) ) ;
#5730 = CARTESIAN_POINT ( 'NONE',  ( -62.26794919243111082, 11.82366454968463110, 0.5000000000000013323 ) ) ;
#5731 = CARTESIAN_POINT ( 'NONE',  ( -61.73205080756886076, 14.44866454968463110, 2.500000000000003109 ) ) ;
#5732 = CARTESIAN_POINT ( 'NONE',  ( 0.5000000000000000000, 0.2499999999999998335, -2.000000000000000000 ) ) ;
#5733 = CARTESIAN_POINT ( 'NONE',  ( -61.13531646874997705, 12.11979166632526628, 1.999225269531026417 ) ) ;
#5734 = CARTESIAN_POINT ( 'NONE',  ( -61.56765823437498852, 15.59895833299193590, 2.248837904296538515 ) ) ;
#5735 = DIRECTION ( 'NONE',  ( -0.000000000000000000, -1.000000000000000000, -0.000000000000000000 ) ) ;
#5736 = CARTESIAN_POINT ( 'NONE',  ( -61.99999999999998579, 16.01562499965860198, 2.498450539062049724 ) ) ;
#5737 = CARTESIAN_POINT ( 'NONE',  ( -62.99999999999998579, 15.82291666598386826, 0.9226497308103756012 ) ) ;
#5738 = DIRECTION ( 'NONE',  ( 0.000000000000000000, 0.000000000000000000, -1.000000000000000000 ) ) ;
#5739 = ORIENTED_EDGE ( 'NONE', *, *, #1348, .T. ) ;
#5740 = AXIS2_PLACEMENT_3D ( 'NONE', #1799, #2690, #903 ) ;
#5741 = CARTESIAN_POINT ( 'NONE',  ( -62.99999999999998579, 11.86458333265053788, 2.077350269189627952 ) ) ;
#5742 = CARTESIAN_POINT ( 'NONE',  ( -61.99999999999998579, 12.43749999999999822, 2.500000000000002665 ) ) ;
#5743 = CARTESIAN_POINT ( 'NONE',  ( -62.43234176562499016, 14.74479166632526805, 2.248837904296538071 ) ) ;
#5744 = CARTESIAN_POINT ( 'NONE',  ( -61.99999999999998579, 10.51562499965860198, 2.498450539062049724 ) ) ;
#5745 = CARTESIAN_POINT ( 'NONE',  ( -62.43234176562498305, 15.22395833299193590, 0.7511620957034662593 ) ) ;
#5746 = CARTESIAN_POINT ( 'NONE',  ( -61.99999999999998579, 15.65624999931720218, 2.500000000000002665 ) ) ;
#5747 = ORIENTED_EDGE ( 'NONE', *, *, #8577, .F. ) ;
#5748 = CARTESIAN_POINT ( 'NONE',  ( -60.99999999999998579, 14.22916666666666785, 2.077350269189628840 ) ) ;
#5749 = CARTESIAN_POINT ( 'NONE',  ( 0.5477065543514070267, 0.000000000000000000, -1.934182851860892116 ) ) ;
#5750 = EDGE_CURVE ( 'NONE', #292, #724, #8668, .T. ) ;
#5751 = CARTESIAN_POINT ( 'NONE',  ( -60.99999999999998579, 12.48958333265053611, 0.9226497308103762673 ) ) ;
#5752 = CARTESIAN_POINT ( 'NONE',  ( -61.73205080756885366, 9.551335450315368902, 0.5000000000000028866 ) ) ;
#5753 = ADVANCED_BREP_SHAPE_REPRESENTATION ( '', ( #8521, #2307 ), #4948 ) ;
#5754 = EDGE_CURVE ( 'NONE', #8509, #4585, #888, .T. ) ;
#5755 = CARTESIAN_POINT ( 'NONE',  ( -61.13531646874998415, 14.55729166632526628, 1.999225269531026417 ) ) ;
#5756 = CARTESIAN_POINT ( 'NONE',  ( -61.99999999999998579, 15.56249999999999822, 0.5000000000000013323 ) ) ;
#5757 = ORIENTED_EDGE ( 'NONE', *, *, #4244, .T. ) ;
#5758 = CARTESIAN_POINT ( 'NONE',  ( -61.13531646874998415, 11.16145833299193413, 1.000774730468978468 ) ) ;
#5759 = CYLINDRICAL_SURFACE ( 'NONE', #4575, 0.9999999999999981126 ) ;
#5760 = DIRECTION ( 'NONE',  ( -0.000000000000000000, 1.000000000000000000, 0.000000000000000000 ) ) ;
#5761 = ORIENTED_EDGE ( 'NONE', *, *, #2457, .F. ) ;
#5762 = CARTESIAN_POINT ( 'NONE',  ( -61.99999999999998579, 11.18750000000000000, 2.500000000000002665 ) ) ;
#5763 = EDGE_CURVE ( 'NONE', #5311, #5466, #3288, .T. ) ;
#5764 =( BOUNDED_CURVE ( )  B_SPLINE_CURVE ( 2, ( #8283, #665, #6572, #7552, #8334, #2285, #723, #5669, #4049 ),
 .UNSPECIFIED., .F., .F. ) 
 B_SPLINE_CURVE_WITH_KNOTS ( ( 3, 2, 2, 2, 3 ),
 ( 0.7890625000000000000, 0.7916666666666666297, 0.7968750000000000000, 0.8020833333333333703, 0.8046875000000000000 ),
 .UNSPECIFIED. ) 
 CURVE ( )  GEOMETRIC_REPRESENTATION_ITEM ( )  RATIONAL_B_SPLINE_CURVE ( ( 0.9330127018922194093, 0.9330127018922194093, 1.000000000000000000, 0.8660254037844387076, 1.000000000000000000, 0.8660254037844387076, 1.000000000000000000, 0.9330127018922194093, 0.9330127018922194093 ) ) 
 REPRESENTATION_ITEM ( '' )  );
#5765 = VERTEX_POINT ( 'NONE', #1726 ) ;
#5766 = DIRECTION ( 'NONE',  ( 1.110223024625156343E-15, 1.000000000000000000, 0.000000000000000000 ) ) ;
#5767 = CARTESIAN_POINT ( 'NONE',  ( -61.99999999999998579, 11.43750000000000000, 2.654700538379254571 ) ) ;
#5768 = CARTESIAN_POINT ( 'NONE',  ( -61.99999999999998579, 16.00000000000000000, 1.500000000000002220 ) ) ;
#5769 = CARTESIAN_POINT ( 'NONE',  ( -61.49999999999998579, 12.20833333333333393, 2.366025403784441927 ) ) ;
#5770 = CARTESIAN_POINT ( 'NONE',  ( -62.99999999999998579, 9.614583332650536107, 2.077350269189627952 ) ) ;
#5771 = CARTESIAN_POINT ( 'NONE',  ( -61.56765823437498142, 11.68229166632526805, 0.7511620957034663704 ) ) ;
#5772 = CARTESIAN_POINT ( 'NONE',  ( -62.49999999999998579, 9.052083332650536107, 0.6339745962155627357 ) ) ;
#5773 = ORIENTED_EDGE ( 'NONE', *, *, #1003, .T. ) ;
#5774 = CARTESIAN_POINT ( 'NONE',  ( -62.26794919243111082, 15.32366454968462932, 0.5000000000000013323 ) ) ;
#5775 = ADVANCED_FACE ( 'NONE', ( #8352 ), #7515, .T. ) ;
#5776 = ORIENTED_EDGE ( 'NONE', *, *, #2597, .F. ) ;
#5777 = LINE ( 'NONE', #3908, #2182 ) ;
#5778 = CARTESIAN_POINT ( 'NONE',  ( -62.43234176562499016, 13.24479166632526805, 2.248837904296538071 ) ) ;
#5779 = CYLINDRICAL_SURFACE ( 'NONE', #6980, 0.9999999999999981126 ) ;
#5780 = CARTESIAN_POINT ( 'NONE',  ( -120.0000000000000000, -8.000000000000000000, 5.000000000000004441 ) ) ;
#5781 = CARTESIAN_POINT ( 'NONE',  ( 0.000000000000000000, 0.000000000000000000, -2.000000000000000000 ) ) ;
#5782 = CARTESIAN_POINT ( 'NONE',  ( -62.86468353124998032, 12.74479166632526805, 1.000774730468978024 ) ) ;
#5783 = CARTESIAN_POINT ( 'NONE',  ( -62.43234176562498305, 15.47395833299193590, 0.7511620957034662593 ) ) ;
#5784 = DIRECTION ( 'NONE',  ( 0.000000000000000000, 0.000000000000000000, 1.000000000000000000 ) ) ;
#5785 = PRODUCT_CONTEXT ( 'NONE', #5555, 'mechanical' ) ;
#5786 = CARTESIAN_POINT ( 'NONE',  ( -61.13531646874998415, 16.07812499965860198, 1.500000000000002220 ) ) ;
#5787 = EDGE_CURVE ( 'NONE', #9306, #1698, #111, .T. ) ;
#5788 = CARTESIAN_POINT ( 'NONE',  ( -61.99999999999998579, 16.03124999931720396, 0.3452994616207497591 ) ) ;
#5789 = CARTESIAN_POINT ( 'NONE',  ( 0.000000000000000000, 0.000000000000000000, 2.000000000000000000 ) ) ;
#5790 = ORIENTED_EDGE ( 'NONE', *, *, #8531, .T. ) ;
#5791 = DIRECTION ( 'NONE',  ( 1.000000000000000000, 0.000000000000000000, 0.000000000000000000 ) ) ;
#5792 = CYLINDRICAL_SURFACE ( 'NONE', #3783, 1.000000000000000888 ) ;
#5793 = CARTESIAN_POINT ( 'NONE',  ( -61.13531646874997705, 14.09895833299193413, 1.000774730468978468 ) ) ;
#5794 = CARTESIAN_POINT ( 'NONE',  ( -62.86468353124998032, 9.682291666325266277, 1.000774730468978246 ) ) ;
#5795 = CARTESIAN_POINT ( 'NONE',  ( -61.13531646874998415, 15.89062499965860198, 1.500000000000002220 ) ) ;
#5796 = CARTESIAN_POINT ( 'NONE',  ( -61.06765823437498852, 8.179687499487902969, 1.500000000000002220 ) ) ;
#5797 = ORIENTED_EDGE ( 'NONE', *, *, #697, .F. ) ;
#5798 = CARTESIAN_POINT ( 'NONE',  ( -62.99999999999998579, 13.37500000000000000, 1.500000000000001998 ) ) ;
#5799 = CARTESIAN_POINT ( 'NONE',  ( -61.13531646874997705, 8.369791666325269830, 1.999225269531026417 ) ) ;
#5800 = SHAPE_REPRESENTATION ( 'depth blade', ( #2307 ), #351 ) ;
#5801 = SURFACE_SIDE_STYLE ('',( #3198 ) ) ;
#5802 = CARTESIAN_POINT ( 'NONE',  ( -60.99999999999998579, 11.48958333265053611, 0.9226497308103762673 ) ) ;
#5803 = CARTESIAN_POINT ( 'NONE',  ( 146.0999999999999943, 5.500000000000000000, 6.000000000000000000 ) ) ;
#5804 = CARTESIAN_POINT ( 'NONE',  ( -61.56765823437498142, 13.36979166632526805, 0.7511620957034663704 ) ) ;
#5805 = SURFACE_STYLE_FILL_AREA ( #3151 ) ;
#5806 = ORIENTED_EDGE ( 'NONE', *, *, #3546, .F. ) ;
#5807 = EDGE_CURVE ( 'NONE', #6146, #4962, #9389, .T. ) ;
#5808 = CARTESIAN_POINT ( 'NONE',  ( -61.13531646874998415, 12.41145833299193413, 1.000774730468978468 ) ) ;
#5809 = DIRECTION ( 'NONE',  ( 0.000000000000000000, 0.000000000000000000, 1.000000000000000000 ) ) ;
#5810 = VECTOR ( 'NONE', #9686, 1000.000000000000000 ) ;
#5811 = UNCERTAINTY_MEASURE_WITH_UNIT (LENGTH_MEASURE( 1.000000000000000082E-05 ), #4733, 'distance_accuracy_value', 'NONE');
#5812 = CARTESIAN_POINT ( 'NONE',  ( 150.0000000000000284, -8.000000000000000000, 3.000000000000000000 ) ) ;
#5813 = EDGE_LOOP ( 'NONE', ( #953, #149, #10092, #5159 ) ) ;
#5814 = CARTESIAN_POINT ( 'NONE',  ( -37.99999999999999289, -14.00000000000000888, -0.9999999999999947820 ) ) ;
#5815=STYLED_ITEM('',(#11034),#4847);
#5816 = EDGE_LOOP ( 'NONE', ( #8147, #2849, #4635, #5936 ) ) ;
#5817 = CARTESIAN_POINT ( 'NONE',  ( -61.49999999999998579, 15.45833333333333393, 2.366025403784441927 ) ) ;
#5818 = CARTESIAN_POINT ( 'NONE',  ( -60.99999999999998579, 11.00000000000000000, 1.500000000000002220 ) ) ;
#5819 = ORIENTED_EDGE ( 'NONE', *, *, #3167, .T. ) ;
#5820 = VECTOR ( 'NONE', #5482, 1000.000000000000000 ) ;
#5821 = CARTESIAN_POINT ( 'NONE',  ( -62.26794919243111082, 13.79241454900183150, 0.5000000000000013323 ) ) ;
#5822 = UNCERTAINTY_MEASURE_WITH_UNIT (LENGTH_MEASURE( 1.000000000000000082E-05 ), #2318, 'distance_accuracy_value', 'NONE');
#5823 = EDGE_CURVE ( 'NONE', #7075, #1330, #5644, .T. ) ;
#5824 = AXIS2_PLACEMENT_3D ( 'NONE', #10387, #5322, #401 ) ;
#5825 = CARTESIAN_POINT ( 'NONE',  ( -61.99999999999998579, 12.57812499965860198, 2.498450539062049724 ) ) ;
#5826 = FACE_BOUND ( 'NONE', #10967, .T. ) ;
#5827 = ORIENTED_EDGE ( 'NONE', *, *, #4446, .T. ) ;
#5828 = DIRECTION ( 'NONE',  ( -0.000000000000000000, -1.000000000000000000, -0.000000000000000000 ) ) ;
#5829 = VECTOR ( 'NONE', #3527, 1000.000000000000000 ) ;
#5830 = EDGE_LOOP ( 'NONE', ( #2087, #7032, #8242, #2564 ) ) ;
#5831 = LINE ( 'NONE', #10051, #10140 ) ;
#5832 = CARTESIAN_POINT ( 'NONE',  ( -61.13531646874998415, 15.57812499965860198, 1.500000000000002220 ) ) ;
#5833 = CIRCLE ( 'NONE', #6729, 1.000000000000000888 ) ;
#5834 = CARTESIAN_POINT ( 'NONE',  ( 145.0000000000000284, -5.500000000000000000, 6.000000000000000000 ) ) ;
#5835 = FACE_OUTER_BOUND ( 'NONE', #2054, .T. ) ;
#5836 = DIRECTION ( 'NONE',  ( -0.000000000000000000, -1.000000000000000000, -0.000000000000000000 ) ) ;
#5837 = CARTESIAN_POINT ( 'NONE',  ( -61.99999999999999289, 12.20312499965860198, 0.5015494609379544944 ) ) ;
#5838 = CARTESIAN_POINT ( 'NONE',  ( -61.99999999999998579, 15.45312499965860020, 0.5015494609379544944 ) ) ;
#5839 =( GEOMETRIC_REPRESENTATION_CONTEXT ( 3 ) GLOBAL_UNCERTAINTY_ASSIGNED_CONTEXT ( ( #9733 ) ) GLOBAL_UNIT_ASSIGNED_CONTEXT ( ( #5978, #204, #9536 ) ) REPRESENTATION_CONTEXT ( 'NONE', 'WORKASPACE' ) );
#5840 = CARTESIAN_POINT ( 'NONE',  ( -62.49999999999998579, 14.38541666598387003, 2.366025403784441483 ) ) ;
#5841 = CARTESIAN_POINT ( 'NONE',  ( -60.99999999999998579, 13.48958333265053611, 0.9226497308103762673 ) ) ;
#5842 = CARTESIAN_POINT ( 'NONE',  ( -62.86468353124998742, 8.536458332991934128, 1.999225269531025972 ) ) ;
#5843 = CARTESIAN_POINT ( 'NONE',  ( -57.99999999999998579, -10.00000000000000888, 3.141811147483251965 ) ) ;
#5844 = ORIENTED_EDGE ( 'NONE', *, *, #8228, .T. ) ;
#5845 = LINE ( 'NONE', #1627, #2831 ) ;
#5846 = CARTESIAN_POINT ( 'NONE',  ( -42.47213595499957961, -10.00000000000000888, 5.000000000000000000 ) ) ;
#5847 = CIRCLE ( 'NONE', #7272, 1.934182851860892116 ) ;
#5848 = AXIS2_PLACEMENT_3D ( 'NONE', #10630, #295, #8143 ) ;
#5849 = CARTESIAN_POINT ( 'NONE',  ( -62.86468353124999453, 14.20312499965860020, 1.500000000000002220 ) ) ;
#5850 = CARTESIAN_POINT ( 'NONE',  ( -61.13531646874998415, 11.55729166632526983, 1.999225269531026417 ) ) ;
#5851 = CARTESIAN_POINT ( 'NONE',  ( -62.86468353124999453, 15.03645833299193590, 1.999225269531025750 ) ) ;
#5852 = FACE_OUTER_BOUND ( 'NONE', #8820, .T. ) ;
#5853 = ORIENTED_EDGE ( 'NONE', *, *, #4946, .F. ) ;
#5854 = CARTESIAN_POINT ( 'NONE',  ( -62.49999999999998579, 13.58333333333333215, 0.6339745962155627357 ) ) ;
#5855 = CARTESIAN_POINT ( 'NONE',  ( -61.13531646874997705, 9.119791666325268054, 1.999225269531026417 ) ) ;
#5856 = AXIS2_PLACEMENT_3D ( 'NONE', #9545, #3775, #7223 ) ;
#5857 = CARTESIAN_POINT ( 'NONE',  ( -62.49999999999998579, 12.05208333265053611, 0.6339745962155627357 ) ) ;
#5858 = PRODUCT_DEFINITION_FORMATION_WITH_SPECIFIED_SOURCE ( 'ANY', '', #10959, .NOT_KNOWN. ) ;
#5859 = VERTEX_POINT ( 'NONE', #9445 ) ;
#5860 = LINE ( 'NONE', #10863, #3588 ) ;
#5861 = CARTESIAN_POINT ( 'NONE',  ( -62.43234176562499016, 13.74479166632526805, 2.248837904296538071 ) ) ;
#5862 = ADVANCED_FACE ( 'NONE', ( #5101 ), #5156, .T. ) ;
#5863 = DIRECTION ( 'NONE',  ( -1.000000000000000000, 0.000000000000000000, -0.000000000000000000 ) ) ;
#5864 =( BOUNDED_CURVE ( )  B_SPLINE_CURVE ( 2, ( #3897, #5663, #1395, #7290, #2281, #4774, #9063, #4824, #620 ),
 .UNSPECIFIED., .F., .F. ) 
 B_SPLINE_CURVE_WITH_KNOTS ( ( 3, 2, 2, 2, 3 ),
 ( 0.8203125000000000000, 0.8229166666666666297, 0.8281250000000000000, 0.8333333333333333703, 0.8359375000000000000 ),
 .UNSPECIFIED. ) 
 CURVE ( )  GEOMETRIC_REPRESENTATION_ITEM ( )  RATIONAL_B_SPLINE_CURVE ( ( 0.9330127018922194093, 0.9330127018922194093, 1.000000000000000000, 0.8660254037844387076, 1.000000000000000000, 0.8660254037844387076, 1.000000000000000000, 0.9330127018922194093, 0.9330127018922194093 ) ) 
 REPRESENTATION_ITEM ( '' )  );
#5865 = VERTEX_POINT ( 'NONE', #10110 ) ;
#5866 = CARTESIAN_POINT ( 'NONE',  ( -61.56765823437498142, 12.43229166632526805, 0.7511620957034663704 ) ) ;
#5867 = DIRECTION ( 'NONE',  ( -0.000000000000000000, -1.000000000000000000, -0.000000000000000000 ) ) ;
#5868 = DIRECTION ( 'NONE',  ( 0.000000000000000000, 0.000000000000000000, 1.000000000000000000 ) ) ;
#5869 = VERTEX_POINT ( 'NONE', #9238 ) ;
#5870 = CARTESIAN_POINT ( 'NONE',  ( -44.00000000000000711, -14.00000000000000888, -0.9999999999999947820 ) ) ;
#5871 = ORIENTED_EDGE ( 'NONE', *, *, #10620, .T. ) ;
#5872 = AXIS2_PLACEMENT_3D ( 'NONE', #10023, #9976, #8362 ) ;
#5873 = CARTESIAN_POINT ( 'NONE',  ( -62.99999999999998579, 11.10416666666666607, 0.9226497308103756012 ) ) ;
#5874 = VERTEX_POINT ( 'NONE', #2561 ) ;
#5875 = CARTESIAN_POINT ( 'NONE',  ( -61.56765823437498852, 9.098958332991935904, 2.248837904296538515 ) ) ;
#5876 = CARTESIAN_POINT ( 'NONE',  ( 146.0999999999999943, -5.500000000000000000, 3.000000000000000888 ) ) ;
#5877 = EDGE_CURVE ( 'NONE', #1190, #4976, #4323, .T. ) ;
#5878 = CARTESIAN_POINT ( 'NONE',  ( -61.99999999999998579, 13.70312499965860198, 0.5015494609379544944 ) ) ;
#5879 = CARTESIAN_POINT ( 'NONE',  ( -62.49999999999998579, 12.05208333265053611, 0.6339745962155627357 ) ) ;
#5880 = VERTEX_POINT ( 'NONE', #835 ) ;
#5881 = VECTOR ( 'NONE', #2510, 1000.000000000000000 ) ;
#5882 = DIRECTION ( 'NONE',  ( -0.000000000000000000, -1.000000000000000000, -0.000000000000000000 ) ) ;
#5883 = ADVANCED_FACE ( 'NONE', ( #5000 ), #944, .F. ) ;
#5884 = ORIENTED_EDGE ( 'NONE', *, *, #153, .F. ) ;
#5885 = DIRECTION ( 'NONE',  ( 0.000000000000000000, -1.000000000000000000, -1.084202172485504434E-16 ) ) ;
#5886 = EDGE_CURVE ( 'NONE', #6102, #8034, #3386, .T. ) ;
#5887 = CARTESIAN_POINT ( 'NONE',  ( -61.13531646874998415, 15.80729166632526628, 1.999225269531026417 ) ) ;
#5888 = CARTESIAN_POINT ( 'NONE',  ( -37.99999999999999289, -14.00000000000000888, 3.000000000000000000 ) ) ;
#5889 = LINE ( 'NONE', #4369, #9739 ) ;
#5890 = CARTESIAN_POINT ( 'NONE',  ( -49.99999999999998579, -4.000000000000019540, 0.000000000000000000 ) ) ;
#5891 = AXIS2_PLACEMENT_3D ( 'NONE', #1938, #5485, #268 ) ;
#5892 = CARTESIAN_POINT ( 'NONE',  ( -61.13531646874998415, 13.39062499965860020, 1.500000000000002220 ) ) ;
#5893 = AXIS2_PLACEMENT_3D ( 'NONE', #6598, #8307, #1481 ) ;
#5894 = CARTESIAN_POINT ( 'NONE',  ( -61.56765823437498142, 8.119791666325268054, 0.7511620957034663704 ) ) ;
#5896 = DIRECTION ( 'NONE',  ( -0.000000000000000000, -1.000000000000000000, -0.000000000000000000 ) ) ;
#5895 = PRODUCT_DEFINITION ( 'UNKNOWN', '', #5858, #9261 ) ;
#5897 = FACE_OUTER_BOUND ( 'NONE', #1761, .T. ) ;
#5898 = CARTESIAN_POINT ( 'NONE',  ( -61.13531646874998415, 9.411458332991934128, 1.000774730468978468 ) ) ;
#5899 = FACE_OUTER_BOUND ( 'NONE', #1905, .T. ) ;
#5900 = VERTEX_POINT ( 'NONE', #8506 ) ;
#5901 = FACE_OUTER_BOUND ( 'NONE', #6795, .T. ) ;
#5902 = CARTESIAN_POINT ( 'NONE',  ( -62.49999999999998579, 12.58333333333333393, 0.6339745962155627357 ) ) ;
#5903 = AXIS2_PLACEMENT_3D ( 'NONE', #7700, #9584, #250 ) ;
#5904 = CARTESIAN_POINT ( 'NONE',  ( -61.99999999999999289, 14.89062499965860020, 0.5015494609379544944 ) ) ;
#5905 = ADVANCED_FACE ( 'NONE', ( #5897 ), #4216, .F. ) ;
#5906 = CARTESIAN_POINT ( 'NONE',  ( -61.56765823437498852, 11.28645833299193590, 2.248837904296538515 ) ) ;
#5907 = CARTESIAN_POINT ( 'NONE',  ( -62.43234176562499016, 15.80729166632526628, 2.248837904296538071 ) ) ;
#5908 = DIRECTION ( 'NONE',  ( 0.000000000000000000, 0.000000000000000000, 1.000000000000000000 ) ) ;
#5909 = VERTEX_POINT ( 'NONE', #7622 ) ;
#5910 = CARTESIAN_POINT ( 'NONE',  ( -61.99999999999998579, 14.56249999999999822, 0.3452994616207497591 ) ) ;
#5911 = CARTESIAN_POINT ( 'NONE',  ( -61.99999999999999289, 8.828124999658601979, 2.498450539062049724 ) ) ;
#5912 = AXIS2_PLACEMENT_3D ( 'NONE', #4209, #10158, #3175 ) ;
#5913 = CARTESIAN_POINT ( 'NONE',  ( -62.99999999999998579, 13.84374999931720218, 1.500000000000001998 ) ) ;
#5914 = ORIENTED_EDGE ( 'NONE', *, *, #703, .F. ) ;
#5915 = DIRECTION ( 'NONE',  ( 0.000000000000000000, 0.000000000000000000, -1.000000000000000000 ) ) ;
#5916 = EDGE_CURVE ( 'NONE', #1996, #1179, #3340, .T. ) ;
#5917 = CARTESIAN_POINT ( 'NONE',  ( -61.13531646874998415, 14.09895833299193413, 1.000774730468978468 ) ) ;
#5918 = FACE_OUTER_BOUND ( 'NONE', #1626, .T. ) ;
#5919 = EDGE_CURVE ( 'NONE', #3055, #9827, #7902, .T. ) ;
#5920 = ORIENTED_EDGE ( 'NONE', *, *, #367, .F. ) ;
#5921 = FACE_OUTER_BOUND ( 'NONE', #5508, .T. ) ;
#5922 = CARTESIAN_POINT ( 'NONE',  ( -62.43234176562498305, 12.47395833299193413, 0.7511620957034662593 ) ) ;
#5923 = CARTESIAN_POINT ( 'NONE',  ( -77.99999999999998579, 0.000000000000000000, 5.000000000000000000 ) ) ;
#5924 = ORIENTED_EDGE ( 'NONE', *, *, #5823, .F. ) ;
#5925 = EDGE_CURVE ( 'NONE', #3366, #41, #5439, .T. ) ;
#5926 = CARTESIAN_POINT ( 'NONE',  ( -61.99999999999998579, 16.00000000000000000, 1.500000000000002220 ) ) ;
#5927 = EDGE_LOOP ( 'NONE', ( #2774, #9168 ) ) ;
#5928 = DIRECTION ( 'NONE',  ( -1.000000000000000000, 0.000000000000000000, 0.000000000000000000 ) ) ;
#5929 =( BOUNDED_SURFACE ( )  B_SPLINE_SURFACE ( 1, 2, ( 
 ( #4718, #6620, #3115, #8125, #458, #3011, #1449, #1397, #513, #622, #3947, #3899, #4000, #9064, #10672, #6462, #4776, #9892, #7395, #198, #4348, #1549, #3273, #85, #6669, #1083, #5241, #4473, #2759, #3471, #10883, #3584, #10241, #1813, #2648, #2586, #7877, #1026, #4931, #3640, #3528, #6089, #7759, #7818, #10000, #720, #8330, #6033, #9475, #6984, #6867, #9417, #140, #2703, #2381, #258, #4410, #4101, #1924, #9165, #1870, #10362, #6145, #10189, #5184, #8592, #5972, #5770, #9530, #7499, #9361, #6930, #8644, #10301, #5297, #1757, #5131, #8535, #972, #8708, #915, #4296, #7706, #1267, #10590, #10415, #8987, #1329, #1983, #9821, #6205, #2989, #4699, #7266, #7932, #6323, #1203, #9706, #311, #2817, #7098, #6376, #7155, #5355, #10537, #3044, #5471, #9590, #8767, #9764, #2043, #1147, #3759, #2158, #2876, #4528, #2097, #3697, #4645, #2936, #8937, #2213, #10479, #5532, #8106, #5592, #6266, #437, #488, #3875, #9652, #8160, #8880, #10649, #5415, #6437, #8050, #1377, #4750, #548, #3821, #7037, #7209, #8819, #4584, #7990, #375, #4908, #10912, #648, #2365, #9039, #7377, #3097, #10028, #4860, #3147, #5802, #6653, #601, #751, #8308, #8210, #5019, #1430, #3251, #4027, #6493, #2410, #9981, #6544, #9199, #7482, #7533, #4807, #9929, #9875, #8418, #4966, #9145, #2261, #3984, #8265, #10756, #5857, #1582, #9251, #3302, #7426, #2315, #8367, #10808, #5643, #4136, #3928, #6698, #700, #10073, #3199, #5698, #9092, #1484, #1532, #2470, #6601, #5751, #4082, #10860, #1639, #7318, #10710, #1911, #5170, #5067, #10123, #10226, #9349, #2575, #6019, #8581, #8632, #8467, #10179, #9302, #6968, #957, #4336, #802, #852, #4179, #902, #1744, #1857, #9515, #3513, #1011, #7581, #4392, #3568, #5961, #5117, #10349, #6808, #2746, #74, #5226, #3459, #7747, #2632, #2522, #9405, #6132, #2689, #5282, #10961, #3350, #8523, #7804, #186, #6753, #7693, #4283, #23, #6074, #6916, #6856, #127, #10285, #9462, #1798, #5913, #1692, #4232, #7639, #3400, #359, #8751, #9805, #2863, #8692, #2974, #7197, #6308, #3032, #9635, #1132, #4514, #10578, #476, #10402, #9690, #243, #3628, #8806, #2029, #7917, #1188, #1311, #2801, #4630, #8922, #298, #7975, #2083, #9576, #6250, #7249, #10462, #5518, #1969, #10632, #1070, #7025, #2145, #8864, #5456, #6424, #3681, #5339, #4686, #8093, #7081, #2200, #4458, #6189, #3860, #1251, #8032, #7860, #5400, #4568, #3745, #7142, #10522, #2922, #422, #3807, #6360, #9748, #2249, #8145, #8197, #10793, #1567, #7306, #532, #5628, #9131, #3183, #9025, #1520, #6684, #9966, #9862, #3916, #4014, #3134, #7360, #6588, #2348, #2397, #1416, #3971, #3082, #736, #5737, #4894, #5578, #4793, #8975, #5686, #6531, #6638, #3289, #8295, #5788, #1366, #9183, #8353, #10745, #9913, #4121, #585, #7516, #4844 ),
 ( #4952, #10899, #7468, #10693, #10061, #682, #4066, #10847, #3231, #4735, #6480, #2302, #1470, #10015, #9079, #8253, #635, #7411, #6001, #5842, #4376, #7733, #8405, #5214, #1624, #9390, #112, #2678, #3334, #1727, #7623, #5102, #6737, #9239, #2509, #1785, #2562, #787, #5949, #9446, #889, #5001, #4166, #5157, #8452, #7567, #10164, #8564, #9288, #10944, #8507, #10111, #8, #1680, #3498, #945, #9335, #10214, #2614, #6899, #4270, #5898, #1843, #5052, #4324, #10270, #7679, #837, #3555, #3388, #2450, #6060, #8618, #61, #7789, #6794, #4217, #3444, #996, #170, #6842, #6952, #1896, #5266, #10445, #280, #6173, #2847, #2960, #1055, #6292, #10562, #10388, #9619, #7958, #228, #4499, #8906, #1117, #7180, #3613, #1293, #2732, #8672, #3789, #10506, #3730, #8077, #9560, #7010, #6344, #4441, #9728, #459, #2124, #7125, #5502, #3666, #2785, #7843, #1954, #4551, #4669, #5323, #8734, #7903, #2905, #340, #7063, #9676, #3843, #2068, #6234, #2012, #8791, #5386, #1173, #5440, #8845, #10332, #1231, #4616, #8016, #6115, #403, #9501, #7233, #7292, #10614, #7342, #8182, #8282, #4933, #9952, #4048, #3012, #10831, #10001, #1399, #4777, #2382, #2232, #9166, #6513, #664, #9893, #10775, #9065, #5562, #4828, #5771, #9114, #569, #10673, #2284, #10732, #7450, #3215, #6621, #3116, #1551, #8332, #3950, #5667, #721, #5612, #6405, #1450, #9790, #8235, #3166, #623, #8960, #4002, #2183, #1503, #7396, #3067, #6570, #2334, #1351, #4719, #8126, #5719, #4879, #6464, #515, #3900, #9846, #9006, #4254, #9375, #5934, #5825, #96, #9222, #2599, #45, #6775, #4152, #5199, #9273, #4102, #1770, #5982, #1712, #9429, #5038, #7551, #10930, #5144, #6881, #1606, #5085, #6670, #10046, #4201, #8436, #3320, #7606, #7718, #4984, #3429, #4309, #6720, #3374, #8490, #8388, #1665, #2662, #3482, #10254, #822, #8545, #6043, #10097, #7661, #929, #1826, #2493, #874, #10200, #8602, #773, #7501, #8345, #6828, #5878, #10884, #9320, #3274, #2432, #10149, #2546, #7941, #267, #1215, #6220, #7771, #2052, #1994, #8001, #8719, #10427, #6100, #4425, #155, #7110, #1937, #209, #2888, #3710, #8654, #8831, #5368, #5251, #2108, #9485, #323, #1097, #3538, #10489, #7047, #3596, #6276, #4537, #4598, #3650, #9661, #2832, #10313, #9601, #10549, #5425, #5309, #7826, #8777, #4483, #384, #3771, #7166, #7889, #6157, #6995, #2944, #6332, #1157, #9715, #5484, #981, #4358, #2716, #6938, #1882, #1037, #10372, #2770, #9542, #9990, #3054, #8892, #3155, #7384, #6501, #3206, #9831, #8947, #4708, #10764, #654, #10599, #9883, #446, #3830, #8996, #2221, #8115, #1386, #1492, #3000, #4816, #9102, #1338, #8169, #2272, #9777, #5600, #6390, #9050, #3991, #2168, #7438, #1276, #7219, #2322, #1439, #5653, #6610, #500, #5543, #4868, #3886, #5705, #2373, #8271 ) ),
 .UNSPECIFIED., .F., .F., .T. ) 
 B_SPLINE_SURFACE_WITH_KNOTS ( ( 2, 2 ),
 ( 3, 2, 2, 2, 2, 2, 2, 2, 2, 2, 2, 2, 2, 2, 2, 2, 2, 2, 2, 2, 2, 2, 2, 2, 2, 2, 2, 2, 2, 2, 2, 2, 2, 2, 2, 2, 2, 2, 2, 2, 2, 2, 2, 2, 2, 2, 2, 2, 2, 2, 2, 2, 2, 2, 2, 2, 2, 2, 2, 2, 2, 2, 2, 2, 2, 2, 2, 2, 2, 2, 2, 2, 2, 2, 2, 2, 2, 2, 2, 2, 2, 2, 2, 2, 2, 2, 2, 2, 2, 2, 2, 2, 2, 2, 2, 2, 2, 2, 2, 2, 2, 2, 2, 2, 2, 2, 2, 2, 2, 2, 2, 2, 2, 2, 2, 2, 2, 2, 2, 2, 2, 2, 2, 2, 2, 2, 2, 2, 2, 2, 2, 2, 2, 2, 2, 2, 2, 2, 2, 2, 2, 2, 2, 2, 2, 2, 2, 2, 2, 2, 2, 2, 2, 2, 2, 2, 2, 2, 2, 2, 2, 2, 2, 2, 2, 2, 2, 2, 2, 2, 2, 2, 2, 2, 2, 2, 2, 2, 2, 2, 2, 2, 2, 2, 2, 2, 2, 2, 2, 2, 2, 2, 3 ),
 ( 0.000000000000000000, 1.000000000000000000 ),
 ( 0.000000000000000000, 0.005208333333333333044, 0.01041666666666666609, 0.01562500000000000000, 0.02083333333333333218, 0.02604166666666666782, 0.03125000000000000000, 0.03645833333333333565, 0.04166666666666666435, 0.04687500000000000000, 0.05208333333333333565, 0.05729166666666666435, 0.06250000000000000000, 0.06770833333333332871, 0.07291666666666667129, 0.07812500000000000000, 0.08333333333333332871, 0.08854166666666667129, 0.09375000000000000000, 0.09895833333333332871, 0.1041666666666666713, 0.1093750000000000000, 0.1145833333333333287, 0.1197916666666666713, 0.1250000000000000000, 0.1302083333333333426, 0.1354166666666666574, 0.1406250000000000000, 0.1458333333333333426, 0.1510416666666666574, 0.1562500000000000000, 0.1614583333333333426, 0.1666666666666666574, 0.1718750000000000000, 0.1770833333333333426, 0.1822916666666666574, 0.1875000000000000000, 0.1927083333333333426, 0.1979166666666666574, 0.2031250000000000000, 0.2083333333333333426, 0.2135416666666666574, 0.2187500000000000000, 0.2239583333333333426, 0.2291666666666666574, 0.2343750000000000000, 0.2395833333333333426, 0.2447916666666666574, 0.2500000000000000000, 0.2552083333333333148, 0.2604166666666666852, 0.2656250000000000000, 0.2708333333333333148, 0.2760416666666666852, 0.2812500000000000000, 0.2864583333333333148, 0.2916666666666666852, 0.2968750000000000000, 0.3020833333333333148, 0.3072916666666666852, 0.3125000000000000000, 0.3177083333333333148, 0.3229166666666666852, 0.3281250000000000000, 0.3333333333333333148, 0.3385416666666666852, 0.3437500000000000000, 0.3489583333333333148, 0.3541666666666666852, 0.3593750000000000000, 0.3645833333333333148, 0.3697916666666666852, 0.3750000000000000000, 0.3802083333333333148, 0.3854166666666666852, 0.3906250000000000000, 0.3958333333333333148, 0.4010416666666666852, 0.4062500000000000000, 0.4114583333333333148, 0.4166666666666666852, 0.4218750000000000000, 0.4270833333333333148, 0.4322916666666666852, 0.4375000000000000000, 0.4427083333333333148, 0.4479166666666666852, 0.4531250000000000000, 0.4583333333333333148, 0.4635416666666666852, 0.4687500000000000000, 0.4739583333333333148, 0.4791666666666666852, 0.4843750000000000000, 0.4895833333333333148, 0.4947916666666666852, 0.5000000000000000000, 0.5052083333333333703, 0.5104166666666666297, 0.5156250000000000000, 0.5208333333333333703, 0.5260416666666666297, 0.5312500000000000000, 0.5364583333333333703, 0.5416666666666666297, 0.5468750000000000000, 0.5520833333333333703, 0.5572916666666666297, 0.5625000000000000000, 0.5677083333333333703, 0.5729166666666666297, 0.5781250000000000000, 0.5833333333333333703, 0.5885416666666666297, 0.5937500000000000000, 0.5989583333333333703, 0.6041666666666666297, 0.6093750000000000000, 0.6145833333333333703, 0.6197916666666666297, 0.6250000000000000000, 0.6302083333333333703, 0.6354166666666666297, 0.6406250000000000000, 0.6458333333333333703, 0.6510416666666666297, 0.6562500000000000000, 0.6614583333333333703, 0.6666666666666666297, 0.6718750000000000000, 0.6770833333333333703, 0.6822916666666666297, 0.6875000000000000000, 0.6927083333333333703, 0.6979166666666666297, 0.7031250000000000000, 0.7083333333333333703, 0.7135416666666666297, 0.7187500000000000000, 0.7239583333333333703, 0.7291666666666666297, 0.7343750000000000000, 0.7395833333333333703, 0.7447916666666666297, 0.7500000000000000000, 0.7552083333333333703, 0.7604166666666666297, 0.7656250000000000000, 0.7708333333333333703, 0.7760416666666666297, 0.7812500000000000000, 0.7864583333333333703, 0.7916666666666666297, 0.7968750000000000000, 0.8020833333333333703, 0.8072916666666666297, 0.8125000000000000000, 0.8177083333333333703, 0.8229166666666666297, 0.8281250000000000000, 0.8333333333333333703, 0.8385416666666666297, 0.8437500000000000000, 0.8489583333333333703, 0.8541666666666666297, 0.8593750000000000000, 0.8645833333333333703, 0.8697916666666666297, 0.8750000000000000000, 0.8802083333333333703, 0.8854166666666666297, 0.8906250000000000000, 0.8958333333333333703, 0.9010416666666666297, 0.9062500000000000000, 0.9114583333333333703, 0.9166666666666666297, 0.9218750000000000000, 0.9270833333333333703, 0.9322916666666666297, 0.9375000000000000000, 0.9427083333333333703, 0.9479166666666666297, 0.9531250000000000000, 0.9583333333333333703, 0.9635416666666666297, 0.9687500000000000000, 0.9739583333333333703, 0.9791666666666666297, 0.9843750000000000000, 0.9895833333333333703, 0.9947916666666666297, 1.000000000000000000 ),
 .UNSPECIFIED. ) 
 GEOMETRIC_REPRESENTATION_ITEM ( )  RATIONAL_B_SPLINE_SURFACE ( (
 ( 1.000000000000000000, 0.8660254037844387076, 1.000000000000000000, 0.8660254037844387076, 1.000000000000000000, 0.8660254037844387076, 1.000000000000000000, 0.8660254037844387076, 1.000000000000000000, 0.8660254037844387076, 1.000000000000000000, 0.8660254037844387076, 1.000000000000000000, 0.8660254037844387076, 1.000000000000000000, 0.8660254037844387076, 1.000000000000000000, 0.8660254037844387076, 1.000000000000000000, 0.8660254037844387076, 1.000000000000000000, 0.8660254037844387076, 1.000000000000000000, 0.8660254037844387076, 1.000000000000000000, 0.8660254037844387076, 1.000000000000000000, 0.8660254037844387076, 1.000000000000000000, 0.8660254037844387076, 1.000000000000000000, 0.8660254037844387076, 1.000000000000000000, 0.8660254037844387076, 1.000000000000000000, 0.8660254037844387076, 1.000000000000000000, 0.8660254037844387076, 1.000000000000000000, 0.8660254037844387076, 1.000000000000000000, 0.8660254037844387076, 1.000000000000000000, 0.8660254037844387076, 1.000000000000000000, 0.8660254037844387076, 1.000000000000000000, 0.8660254037844387076, 1.000000000000000000, 0.8660254037844387076, 1.000000000000000000, 0.8660254037844387076, 1.000000000000000000, 0.8660254037844387076, 1.000000000000000000, 0.8660254037844387076, 1.000000000000000000, 0.8660254037844387076, 1.000000000000000000, 0.8660254037844387076, 1.000000000000000000, 0.8660254037844387076, 1.000000000000000000, 0.8660254037844387076, 1.000000000000000000, 0.8660254037844387076, 1.000000000000000000, 0.8660254037844387076, 1.000000000000000000, 0.8660254037844387076, 1.000000000000000000, 0.8660254037844387076, 1.000000000000000000, 0.8660254037844387076, 1.000000000000000000, 0.8660254037844387076, 1.000000000000000000, 0.8660254037844387076, 1.000000000000000000, 0.8660254037844387076, 1.000000000000000000, 0.8660254037844387076, 1.000000000000000000, 0.8660254037844387076, 1.000000000000000000, 0.8660254037844387076, 1.000000000000000000, 0.8660254037844387076, 1.000000000000000000, 0.8660254037844387076, 1.000000000000000000, 0.8660254037844387076, 1.000000000000000000, 0.8660254037844387076, 1.000000000000000000, 0.8660254037844387076, 1.000000000000000000, 0.8660254037844387076, 1.000000000000000000, 0.8660254037844387076, 1.000000000000000000, 0.8660254037844387076, 1.000000000000000000, 0.8660254037844387076, 1.000000000000000000, 0.8660254037844387076, 1.000000000000000000, 0.8660254037844387076, 1.000000000000000000, 0.8660254037844387076, 1.000000000000000000, 0.8660254037844387076, 1.000000000000000000, 0.8660254037844387076, 1.000000000000000000, 0.8660254037844387076, 1.000000000000000000, 0.8660254037844387076, 1.000000000000000000, 0.8660254037844387076, 1.000000000000000000, 0.8660254037844387076, 1.000000000000000000, 0.8660254037844387076, 1.000000000000000000, 0.8660254037844387076, 1.000000000000000000, 0.8660254037844387076, 1.000000000000000000, 0.8660254037844387076, 1.000000000000000000, 0.8660254037844387076, 1.000000000000000000, 0.8660254037844387076, 1.000000000000000000, 0.8660254037844387076, 1.000000000000000000, 0.8660254037844387076, 1.000000000000000000, 0.8660254037844387076, 1.000000000000000000, 0.8660254037844387076, 1.000000000000000000, 0.8660254037844387076, 1.000000000000000000, 0.8660254037844387076, 1.000000000000000000, 0.8660254037844387076, 1.000000000000000000, 0.8660254037844387076, 1.000000000000000000, 0.8660254037844387076, 1.000000000000000000, 0.8660254037844387076, 1.000000000000000000, 0.8660254037844387076, 1.000000000000000000, 0.8660254037844387076, 1.000000000000000000, 0.8660254037844387076, 1.000000000000000000, 0.8660254037844387076, 1.000000000000000000, 0.8660254037844387076, 1.000000000000000000, 0.8660254037844387076, 1.000000000000000000, 0.8660254037844387076, 1.000000000000000000, 0.8660254037844387076, 1.000000000000000000, 0.8660254037844387076, 1.000000000000000000, 0.8660254037844387076, 1.000000000000000000, 0.8660254037844387076, 1.000000000000000000, 0.8660254037844387076, 1.000000000000000000, 0.8660254037844387076, 1.000000000000000000, 0.8660254037844387076, 1.000000000000000000, 0.8660254037844387076, 1.000000000000000000, 0.8660254037844387076, 1.000000000000000000, 0.8660254037844387076, 1.000000000000000000, 0.8660254037844387076, 1.000000000000000000, 0.8660254037844387076, 1.000000000000000000, 0.8660254037844387076, 1.000000000000000000, 0.8660254037844387076, 1.000000000000000000, 0.8660254037844387076, 1.000000000000000000, 0.8660254037844387076, 1.000000000000000000, 0.8660254037844387076, 1.000000000000000000, 0.8660254037844387076, 1.000000000000000000, 0.8660254037844387076, 1.000000000000000000, 0.8660254037844387076, 1.000000000000000000, 0.8660254037844387076, 1.000000000000000000, 0.8660254037844387076, 1.000000000000000000, 0.8660254037844387076, 1.000000000000000000, 0.8660254037844387076, 1.000000000000000000, 0.8660254037844387076, 1.000000000000000000, 0.8660254037844387076, 1.000000000000000000, 0.8660254037844387076, 1.000000000000000000, 0.8660254037844387076, 1.000000000000000000, 0.8660254037844387076, 1.000000000000000000, 0.8660254037844387076, 1.000000000000000000, 0.8660254037844387076, 1.000000000000000000, 0.8660254037844387076, 1.000000000000000000, 0.8660254037844387076, 1.000000000000000000, 0.8660254037844387076, 1.000000000000000000, 0.8660254037844387076, 1.000000000000000000, 0.8660254037844387076, 1.000000000000000000, 0.8660254037844387076, 1.000000000000000000, 0.8660254037844387076, 1.000000000000000000, 0.8660254037844387076, 1.000000000000000000, 0.8660254037844387076, 1.000000000000000000, 0.8660254037844387076, 1.000000000000000000, 0.8660254037844387076, 1.000000000000000000, 0.8660254037844387076, 1.000000000000000000, 0.8660254037844387076, 1.000000000000000000, 0.8660254037844387076, 1.000000000000000000, 0.8660254037844387076, 1.000000000000000000, 0.8660254037844387076, 1.000000000000000000, 0.8660254037844387076, 1.000000000000000000, 0.8660254037844387076, 1.000000000000000000, 0.8660254037844387076, 1.000000000000000000, 0.8660254037844387076, 1.000000000000000000, 0.8660254037844387076, 1.000000000000000000, 0.8660254037844387076, 1.000000000000000000, 0.8660254037844387076, 1.000000000000000000, 0.8660254037844387076, 1.000000000000000000, 0.8660254037844387076, 1.000000000000000000, 0.8660254037844387076, 1.000000000000000000, 0.8660254037844387076, 1.000000000000000000, 0.8660254037844387076, 1.000000000000000000, 0.8660254037844387076, 1.000000000000000000, 0.8660254037844387076, 1.000000000000000000, 0.8660254037844387076, 1.000000000000000000, 0.8660254037844387076, 1.000000000000000000, 0.8660254037844387076, 1.000000000000000000, 0.8660254037844387076, 1.000000000000000000, 0.8660254037844387076, 1.000000000000000000, 0.8660254037844387076, 1.000000000000000000, 0.8660254037844387076, 1.000000000000000000, 0.8660254037844387076, 1.000000000000000000, 0.8660254037844387076, 1.000000000000000000, 0.8660254037844387076, 1.000000000000000000, 0.8660254037844387076, 1.000000000000000000, 0.8660254037844387076, 1.000000000000000000, 0.8660254037844387076, 1.000000000000000000, 0.8660254037844387076, 1.000000000000000000, 0.8660254037844387076, 1.000000000000000000, 0.8660254037844387076, 1.000000000000000000, 0.8660254037844387076, 1.000000000000000000, 0.8660254037844387076, 1.000000000000000000, 0.8660254037844387076, 1.000000000000000000, 0.8660254037844387076, 1.000000000000000000, 0.8660254037844387076, 1.000000000000000000, 0.8660254037844387076, 1.000000000000000000, 0.8660254037844387076, 1.000000000000000000, 0.8660254037844387076, 1.000000000000000000, 0.8660254037844387076, 1.000000000000000000, 0.8660254037844387076, 1.000000000000000000, 0.8660254037844387076, 1.000000000000000000, 0.8660254037844387076, 1.000000000000000000, 0.8660254037844387076, 1.000000000000000000, 0.8660254037844387076, 1.000000000000000000, 0.8660254037844387076, 1.000000000000000000, 0.8660254037844387076, 1.000000000000000000, 0.8660254037844387076, 1.000000000000000000, 0.8660254037844387076, 1.000000000000000000, 0.8660254037844387076, 1.000000000000000000, 0.8660254037844387076, 1.000000000000000000, 0.8660254037844387076, 1.000000000000000000, 0.8660254037844387076, 1.000000000000000000, 0.8660254037844387076, 1.000000000000000000, 0.8660254037844387076, 1.000000000000000000, 0.8660254037844387076, 1.000000000000000000, 0.8660254037844387076, 1.000000000000000000, 0.8660254037844387076, 1.000000000000000000, 0.8660254037844387076, 1.000000000000000000, 0.8660254037844387076, 1.000000000000000000, 0.8660254037844387076, 1.000000000000000000, 0.8660254037844387076, 1.000000000000000000),
 ( 1.000000000000000000, 0.8660254037844387076, 1.000000000000000000, 0.8660254037844387076, 1.000000000000000000, 0.8660254037844387076, 1.000000000000000000, 0.8660254037844387076, 1.000000000000000000, 0.8660254037844387076, 1.000000000000000000, 0.8660254037844387076, 1.000000000000000000, 0.8660254037844387076, 1.000000000000000000, 0.8660254037844387076, 1.000000000000000000, 0.8660254037844387076, 1.000000000000000000, 0.8660254037844387076, 1.000000000000000000, 0.8660254037844387076, 1.000000000000000000, 0.8660254037844387076, 1.000000000000000000, 0.8660254037844387076, 1.000000000000000000, 0.8660254037844387076, 1.000000000000000000, 0.8660254037844387076, 1.000000000000000000, 0.8660254037844387076, 1.000000000000000000, 0.8660254037844387076, 1.000000000000000000, 0.8660254037844387076, 1.000000000000000000, 0.8660254037844387076, 1.000000000000000000, 0.8660254037844387076, 1.000000000000000000, 0.8660254037844387076, 1.000000000000000000, 0.8660254037844387076, 1.000000000000000000, 0.8660254037844387076, 1.000000000000000000, 0.8660254037844387076, 1.000000000000000000, 0.8660254037844387076, 1.000000000000000000, 0.8660254037844387076, 1.000000000000000000, 0.8660254037844387076, 1.000000000000000000, 0.8660254037844387076, 1.000000000000000000, 0.8660254037844387076, 1.000000000000000000, 0.8660254037844387076, 1.000000000000000000, 0.8660254037844387076, 1.000000000000000000, 0.8660254037844387076, 1.000000000000000000, 0.8660254037844387076, 1.000000000000000000, 0.8660254037844387076, 1.000000000000000000, 0.8660254037844387076, 1.000000000000000000, 0.8660254037844387076, 1.000000000000000000, 0.8660254037844387076, 1.000000000000000000, 0.8660254037844387076, 1.000000000000000000, 0.8660254037844387076, 1.000000000000000000, 0.8660254037844387076, 1.000000000000000000, 0.8660254037844387076, 1.000000000000000000, 0.8660254037844387076, 1.000000000000000000, 0.8660254037844387076, 1.000000000000000000, 0.8660254037844387076, 1.000000000000000000, 0.8660254037844387076, 1.000000000000000000, 0.8660254037844387076, 1.000000000000000000, 0.8660254037844387076, 1.000000000000000000, 0.8660254037844387076, 1.000000000000000000, 0.8660254037844387076, 1.000000000000000000, 0.8660254037844387076, 1.000000000000000000, 0.8660254037844387076, 1.000000000000000000, 0.8660254037844387076, 1.000000000000000000, 0.8660254037844387076, 1.000000000000000000, 0.8660254037844387076, 1.000000000000000000, 0.8660254037844387076, 1.000000000000000000, 0.8660254037844387076, 1.000000000000000000, 0.8660254037844387076, 1.000000000000000000, 0.8660254037844387076, 1.000000000000000000, 0.8660254037844387076, 1.000000000000000000, 0.8660254037844387076, 1.000000000000000000, 0.8660254037844387076, 1.000000000000000000, 0.8660254037844387076, 1.000000000000000000, 0.8660254037844387076, 1.000000000000000000, 0.8660254037844387076, 1.000000000000000000, 0.8660254037844387076, 1.000000000000000000, 0.8660254037844387076, 1.000000000000000000, 0.8660254037844387076, 1.000000000000000000, 0.8660254037844387076, 1.000000000000000000, 0.8660254037844387076, 1.000000000000000000, 0.8660254037844387076, 1.000000000000000000, 0.8660254037844387076, 1.000000000000000000, 0.8660254037844387076, 1.000000000000000000, 0.8660254037844387076, 1.000000000000000000, 0.8660254037844387076, 1.000000000000000000, 0.8660254037844387076, 1.000000000000000000, 0.8660254037844387076, 1.000000000000000000, 0.8660254037844387076, 1.000000000000000000, 0.8660254037844387076, 1.000000000000000000, 0.8660254037844387076, 1.000000000000000000, 0.8660254037844387076, 1.000000000000000000, 0.8660254037844387076, 1.000000000000000000, 0.8660254037844387076, 1.000000000000000000, 0.8660254037844387076, 1.000000000000000000, 0.8660254037844387076, 1.000000000000000000, 0.8660254037844387076, 1.000000000000000000, 0.8660254037844387076, 1.000000000000000000, 0.8660254037844387076, 1.000000000000000000, 0.8660254037844387076, 1.000000000000000000, 0.8660254037844387076, 1.000000000000000000, 0.8660254037844387076, 1.000000000000000000, 0.8660254037844387076, 1.000000000000000000, 0.8660254037844387076, 1.000000000000000000, 0.8660254037844387076, 1.000000000000000000, 0.8660254037844387076, 1.000000000000000000, 0.8660254037844387076, 1.000000000000000000, 0.8660254037844387076, 1.000000000000000000, 0.8660254037844387076, 1.000000000000000000, 0.8660254037844387076, 1.000000000000000000, 0.8660254037844387076, 1.000000000000000000, 0.8660254037844387076, 1.000000000000000000, 0.8660254037844387076, 1.000000000000000000, 0.8660254037844387076, 1.000000000000000000, 0.8660254037844387076, 1.000000000000000000, 0.8660254037844387076, 1.000000000000000000, 0.8660254037844387076, 1.000000000000000000, 0.8660254037844387076, 1.000000000000000000, 0.8660254037844387076, 1.000000000000000000, 0.8660254037844387076, 1.000000000000000000, 0.8660254037844387076, 1.000000000000000000, 0.8660254037844387076, 1.000000000000000000, 0.8660254037844387076, 1.000000000000000000, 0.8660254037844387076, 1.000000000000000000, 0.8660254037844387076, 1.000000000000000000, 0.8660254037844387076, 1.000000000000000000, 0.8660254037844387076, 1.000000000000000000, 0.8660254037844387076, 1.000000000000000000, 0.8660254037844387076, 1.000000000000000000, 0.8660254037844387076, 1.000000000000000000, 0.8660254037844387076, 1.000000000000000000, 0.8660254037844387076, 1.000000000000000000, 0.8660254037844387076, 1.000000000000000000, 0.8660254037844387076, 1.000000000000000000, 0.8660254037844387076, 1.000000000000000000, 0.8660254037844387076, 1.000000000000000000, 0.8660254037844387076, 1.000000000000000000, 0.8660254037844387076, 1.000000000000000000, 0.8660254037844387076, 1.000000000000000000, 0.8660254037844387076, 1.000000000000000000, 0.8660254037844387076, 1.000000000000000000, 0.8660254037844387076, 1.000000000000000000, 0.8660254037844387076, 1.000000000000000000, 0.8660254037844387076, 1.000000000000000000, 0.8660254037844387076, 1.000000000000000000, 0.8660254037844387076, 1.000000000000000000, 0.8660254037844387076, 1.000000000000000000, 0.8660254037844387076, 1.000000000000000000, 0.8660254037844387076, 1.000000000000000000, 0.8660254037844387076, 1.000000000000000000, 0.8660254037844387076, 1.000000000000000000, 0.8660254037844387076, 1.000000000000000000, 0.8660254037844387076, 1.000000000000000000, 0.8660254037844387076, 1.000000000000000000, 0.8660254037844387076, 1.000000000000000000, 0.8660254037844387076, 1.000000000000000000, 0.8660254037844387076, 1.000000000000000000, 0.8660254037844387076, 1.000000000000000000, 0.8660254037844387076, 1.000000000000000000, 0.8660254037844387076, 1.000000000000000000, 0.8660254037844387076, 1.000000000000000000, 0.8660254037844387076, 1.000000000000000000, 0.8660254037844387076, 1.000000000000000000, 0.8660254037844387076, 1.000000000000000000, 0.8660254037844387076, 1.000000000000000000, 0.8660254037844387076, 1.000000000000000000, 0.8660254037844387076, 1.000000000000000000, 0.8660254037844387076, 1.000000000000000000, 0.8660254037844387076, 1.000000000000000000, 0.8660254037844387076, 1.000000000000000000, 0.8660254037844387076, 1.000000000000000000, 0.8660254037844387076, 1.000000000000000000, 0.8660254037844387076, 1.000000000000000000, 0.8660254037844387076, 1.000000000000000000, 0.8660254037844387076, 1.000000000000000000, 0.8660254037844387076, 1.000000000000000000, 0.8660254037844387076, 1.000000000000000000, 0.8660254037844387076, 1.000000000000000000, 0.8660254037844387076, 1.000000000000000000, 0.8660254037844387076, 1.000000000000000000, 0.8660254037844387076, 1.000000000000000000, 0.8660254037844387076, 1.000000000000000000, 0.8660254037844387076, 1.000000000000000000, 0.8660254037844387076, 1.000000000000000000, 0.8660254037844387076, 1.000000000000000000, 0.8660254037844387076, 1.000000000000000000, 0.8660254037844387076, 1.000000000000000000, 0.8660254037844387076, 1.000000000000000000, 0.8660254037844387076, 1.000000000000000000, 0.8660254037844387076, 1.000000000000000000, 0.8660254037844387076, 1.000000000000000000, 0.8660254037844387076, 1.000000000000000000, 0.8660254037844387076, 1.000000000000000000, 0.8660254037844387076, 1.000000000000000000, 0.8660254037844387076, 1.000000000000000000, 0.8660254037844387076, 1.000000000000000000, 0.8660254037844387076, 1.000000000000000000, 0.8660254037844387076, 1.000000000000000000, 0.8660254037844387076, 1.000000000000000000, 0.8660254037844387076, 1.000000000000000000, 0.8660254037844387076, 1.000000000000000000, 0.8660254037844387076, 1.000000000000000000, 0.8660254037844387076, 1.000000000000000000, 0.8660254037844387076, 1.000000000000000000) ) ) 
 REPRESENTATION_ITEM ( '' )  SURFACE ( )  );
#5930 = ORIENTED_EDGE ( 'NONE', *, *, #4471, .F. ) ;
#5931 = VERTEX_POINT ( 'NONE', #2783 ) ;
#5932 = CARTESIAN_POINT ( 'NONE',  ( -61.99999999999998579, 9.578124999658601979, 2.498450539062049724 ) ) ;
#5933 = CARTESIAN_POINT ( 'NONE',  ( -105.0000000000000000, -2.500000000000000000, 4.000000000000000000 ) ) ;
#5934 = CARTESIAN_POINT ( 'NONE',  ( -62.43234176562499016, 12.55729166632526805, 2.248837904296538071 ) ) ;
#5935 = CARTESIAN_POINT ( 'NONE',  ( -62.99999999999998579, 12.86458333265053611, 2.077350269189627952 ) ) ;
#5936 = ORIENTED_EDGE ( 'NONE', *, *, #3812, .T. ) ;
#5937 = CARTESIAN_POINT ( 'NONE',  ( -49.99999999999998579, -15.00000000000001066, 0.000000000000000000 ) ) ;
#5938 = ORIENTED_EDGE ( 'NONE', *, *, #6880, .F. ) ;
#5939 = CARTESIAN_POINT ( 'NONE',  ( -62.49999999999998579, 11.55208333265053611, 0.6339745962155627357 ) ) ;
#5940 = CARTESIAN_POINT ( 'NONE',  ( -61.13531646874998415, 15.55729166632526628, 1.999225269531026417 ) ) ;
#5941 = FACE_OUTER_BOUND ( 'NONE', #4132, .T. ) ;
#5942 = DIRECTION ( 'NONE',  ( 0.000000000000000000, 0.000000000000000000, -1.000000000000000000 ) ) ;
#5943 = DIRECTION ( 'NONE',  ( 1.000000000000000000, 0.000000000000000000, 0.000000000000000000 ) ) ;
#5944 = CARTESIAN_POINT ( 'NONE',  ( -61.56765823437498142, 13.18229166632526805, 0.7511620957034663704 ) ) ;
#5945 = CARTESIAN_POINT ( 'NONE',  ( -61.99999999999998579, 8.765624999658601979, 2.498450539062049724 ) ) ;
#5946 = EDGE_CURVE ( 'NONE', #1996, #2937, #2629, .T. ) ;
#5947 = DIRECTION ( 'NONE',  ( -0.000000000000000000, -0.000000000000000000, -1.000000000000000000 ) ) ;
#5948 = DIRECTION ( 'NONE',  ( 1.000000000000000000, 0.000000000000000000, 0.000000000000000000 ) ) ;
#5949 = CARTESIAN_POINT ( 'NONE',  ( -61.56765823437498142, 8.932291666325268054, 0.7511620957034663704 ) ) ;
#5950 = DIRECTION ( 'NONE',  ( 0.000000000000000000, 0.000000000000000000, -1.000000000000000000 ) ) ;
#5951 = ORIENTED_EDGE ( 'NONE', *, *, #3403, .T. ) ;
#5952 = PLANE ( 'NONE',  #6742 ) ;
#5953 = LINE ( 'NONE', #9505, #2006 ) ;
#5954 = CARTESIAN_POINT ( 'NONE',  ( -61.56765823437498142, 15.61979166632526628, 0.7511620957034663704 ) ) ;
#5955 = CARTESIAN_POINT ( 'NONE',  ( -62.43234176562499016, 11.49479166632526805, 2.248837904296538071 ) ) ;
#5956 = CARTESIAN_POINT ( 'NONE',  ( -61.13531646874998415, 15.14062499965860020, 1.500000000000002220 ) ) ;
#5957 = CARTESIAN_POINT ( 'NONE',  ( -62.99999999999998579, 13.11458333265053433, 2.077350269189627952 ) ) ;
#5958 = ORIENTED_EDGE ( 'NONE', *, *, #6504, .T. ) ;
#5959 = CARTESIAN_POINT ( 'NONE',  ( -62.99999999999998579, 15.60416666666666607, 0.9226497308103756012 ) ) ;
#5960 = CARTESIAN_POINT ( 'NONE',  ( -62.43234176562498305, 8.973958332991934128, 0.7511620957034662593 ) ) ;
#5961 = CARTESIAN_POINT ( 'NONE',  ( -60.99999999999998579, 13.19791666598386826, 2.077350269189628840 ) ) ;
#5962 = LINE ( 'NONE', #6133, #4666 ) ;
#5963 = ADVANCED_FACE ( 'NONE', ( #6951 ), #3788, .F. ) ;
#5964 = FACE_OUTER_BOUND ( 'NONE', #9758, .T. ) ;
#5965 = CARTESIAN_POINT ( 'NONE',  ( -61.56765823437498852, 11.53645833299193590, 2.248837904296538515 ) ) ;
#5966 = CARTESIAN_POINT ( 'NONE',  ( -62.26794919243111082, 15.67633545031536713, 2.500000000000003109 ) ) ;
#5967 = EDGE_LOOP ( 'NONE', ( #8547, #7012, #1153, #1084, #5194, #998, #3541, #8117 ) ) ;
#5968 = CARTESIAN_POINT ( 'NONE',  ( -62.99999999999998579, 12.87500000000000178, 1.500000000000001998 ) ) ;
#5969 = CARTESIAN_POINT ( 'NONE',  ( -62.43234176562498305, 13.22395833299193413, 0.7511620957034662593 ) ) ;
#5970 = SURFACE_STYLE_FILL_AREA ( #5351 ) ;
#5971 = CARTESIAN_POINT ( 'NONE',  ( 140.0000000000000284, -8.000000000000000000, 6.000000000000000000 ) ) ;
#5972 = CARTESIAN_POINT ( 'NONE',  ( -62.99999999999998579, 9.593749999317202182, 1.500000000000001998 ) ) ;
#5973 = ORIENTED_EDGE ( 'NONE', *, *, #2902, .F. ) ;
#5974 = LINE ( 'NONE', #5812, #10451 ) ;
#5975 = VERTEX_POINT ( 'NONE', #9675 ) ;
#5976 = CARTESIAN_POINT ( 'NONE',  ( -60.99999999999998579, 14.77083333333333215, 0.9226497308103762673 ) ) ;
#5977 = CARTESIAN_POINT ( 'NONE',  ( -61.13531646874998415, 11.55729166632526983, 1.999225269531026417 ) ) ;
#5978 =( LENGTH_UNIT ( ) NAMED_UNIT ( * ) SI_UNIT ( .MILLI., .METRE. ) );
#5979 = ORIENTED_EDGE ( 'NONE', *, *, #4707, .T. ) ;
#5980 = CARTESIAN_POINT ( 'NONE',  ( -61.99999999999998579, 9.078124999658601979, 2.498450539062049724 ) ) ;
#5981 = CARTESIAN_POINT ( 'NONE',  ( -61.73205080756886076, 14.19866454968462932, 2.500000000000003109 ) ) ;
#5982 = CARTESIAN_POINT ( 'NONE',  ( -62.43234176562499016, 12.80729166632526805, 2.248837904296538071 ) ) ;
#5983 = CARTESIAN_POINT ( 'NONE',  ( -61.49999999999998579, 13.20833333333333215, 2.366025403784441927 ) ) ;
#5984 = ORIENTED_EDGE ( 'NONE', *, *, #4052, .T. ) ;
#5985 =( BOUNDED_CURVE ( )  B_SPLINE_CURVE ( 2, ( #79, #1976, #5346, #3465, #6315, #8982, #9813, #9869, #6432 ),
 .UNSPECIFIED., .F., .T. ) 
 B_SPLINE_CURVE_WITH_KNOTS ( ( 3, 2, 2, 2, 3 ),
 ( 0.03906250000000002082, 0.04166666666666666435, 0.04687500000000000000, 0.05208333333333333565, 0.05468749999999997918 ),
 .UNSPECIFIED. ) 
 CURVE ( )  GEOMETRIC_REPRESENTATION_ITEM ( )  RATIONAL_B_SPLINE_CURVE ( ( 0.9330127018922192983, 0.9330127018922198534, 1.000000000000000000, 0.8660254037844387076, 1.000000000000000000, 0.8660254037844387076, 1.000000000000000000, 0.9330127018922198534, 0.9330127018922192983 ) ) 
 REPRESENTATION_ITEM ( '' )  );
#5986 = CARTESIAN_POINT ( 'NONE',  ( -79.09999999999999432, 11.49999999999999645, 4.999999999999999112 ) ) ;
#5987 = AXIS2_PLACEMENT_3D ( 'NONE', #8089, #4563, #8917 ) ;
#5988 = PRODUCT_DEFINITION_SHAPE ( 'NONE', 'NONE',  #10985 ) ;
#5989 = VECTOR ( 'NONE', #4357, 1000.000000000000000 ) ;
#5990 = VERTEX_POINT ( 'NONE', #10331 ) ;
#5991 = CARTESIAN_POINT ( 'NONE',  ( -42.47213595499957961, -10.00000000000000888, 0.000000000000000000 ) ) ;
#5992 = ADVANCED_FACE ( 'NONE', ( #7788 ), #4941, .F. ) ;
#5993 = CARTESIAN_POINT ( 'NONE',  ( -62.86468353124999453, 15.20312499965860020, 1.500000000000002220 ) ) ;
#5994 = CARTESIAN_POINT ( 'NONE',  ( -62.26794919243111082, 9.926335450315368902, 2.500000000000003109 ) ) ;
#5995 = CARTESIAN_POINT ( 'NONE',  ( -114.9999999999999289, -15.00000000000001421, 5.000000000000004441 ) ) ;
#5996 = CARTESIAN_POINT ( 'NONE',  ( -78.99999999999998579, -11.50000000000000711, 5.000000000000000000 ) ) ;
#5997 = CARTESIAN_POINT ( 'NONE',  ( -61.99999999999999289, 14.70312499965860020, 0.5015494609379544944 ) ) ;
#5998 = CARTESIAN_POINT ( 'NONE',  ( -62.86468353124998032, 8.932291666325268054, 1.000774730468978246 ) ) ;
#5999 = CARTESIAN_POINT ( 'NONE',  ( -104.9999999999999289, -16.54248688935409106, 0.000000000000000000 ) ) ;
#6000 = DIRECTION ( 'NONE',  ( -0.000000000000000000, -0.000000000000000000, -1.000000000000000000 ) ) ;
#6001 = CARTESIAN_POINT ( 'NONE',  ( -62.86468353124999453, 8.515624999658601979, 1.500000000000002220 ) ) ;
#6002 = VECTOR ( 'NONE', #2782, 1000.000000000000000 ) ;
#6003 = PLANE ( 'NONE',  #390 ) ;
#6004 = VERTEX_POINT ( 'NONE', #8843 ) ;
#6005 = DIRECTION ( 'NONE',  ( -0.000000000000000000, 1.000000000000000000, 0.000000000000000000 ) ) ;
#6006 = CARTESIAN_POINT ( 'NONE',  ( -61.99999999999998579, 11.15624999931720218, 2.500000000000002665 ) ) ;
#6007 = VECTOR ( 'NONE', #3443, 1000.000000000000000 ) ;
#6008 = ADVANCED_FACE ( 'NONE', ( #8732, #995 ), #2904, .T. ) ;
#6009 = CARTESIAN_POINT ( 'NONE',  ( -61.56765823437498852, 15.28645833299193590, 2.248837904296538515 ) ) ;
#6010 = CARTESIAN_POINT ( 'NONE',  ( -61.99999999999998579, 11.39062499965859843, 0.5015494609379544944 ) ) ;
#6011 = CARTESIAN_POINT ( 'NONE',  ( -61.99999999999999289, 8.765624999658601979, 2.498450539062049724 ) ) ;
#6012 =( GEOMETRIC_REPRESENTATION_CONTEXT ( 3 ) GLOBAL_UNCERTAINTY_ASSIGNED_CONTEXT ( ( #8850 ) ) GLOBAL_UNIT_ASSIGNED_CONTEXT ( ( #3469, #5182, #6087 ) ) REPRESENTATION_CONTEXT ( 'NONE', 'WORKASPACE' ) );
#6013 = CARTESIAN_POINT ( 'NONE',  ( -61.49999999999998579, 9.760416665983870033, 0.6339745962155628467 ) ) ;
#6014 = ORIENTED_EDGE ( 'NONE', *, *, #2042, .F. ) ;
#6015 = CARTESIAN_POINT ( 'NONE',  ( -62.49999999999998579, 15.66666666666666607, 2.366025403784441483 ) ) ;
#6016 = CARTESIAN_POINT ( 'NONE',  ( -61.56765823437498142, 8.682291666325268054, 0.7511620957034663704 ) ) ;
#6017 = DIRECTION ( 'NONE',  ( 1.000000000000000000, 0.000000000000000000, 0.000000000000000000 ) ) ;
#6018 = VECTOR ( 'NONE', #6740, 1000.000000000000000 ) ;
#6019 = CARTESIAN_POINT ( 'NONE',  ( -61.49999999999998579, 12.76041666598386826, 0.6339745962155628467 ) ) ;
#6020 = LINE ( 'NONE', #187, #10533 ) ;
#6021 = ORIENTED_EDGE ( 'NONE', *, *, #9712, .F. ) ;
#6022 = DIRECTION ( 'NONE',  ( 1.000000000000000000, 0.000000000000000000, 0.000000000000000000 ) ) ;
#6023 = EDGE_CURVE ( 'NONE', #4618, #5618, #3729, .T. ) ;
#6024 = CARTESIAN_POINT ( 'NONE',  ( -62.86468353124999453, 11.45312499965860020, 1.500000000000002220 ) ) ;
#6025 = CARTESIAN_POINT ( 'NONE',  ( -49.99999999999998579, -15.00000000000001243, 3.000000000000002665 ) ) ;
#6026 = VECTOR ( 'NONE', #1218, 1000.000000000000000 ) ;
#6027 = DIRECTION ( 'NONE',  ( 0.000000000000000000, 0.000000000000000000, 1.000000000000000000 ) ) ;
#6028 = ORIENTED_EDGE ( 'NONE', *, *, #9696, .T. ) ;
#6029 = ADVANCED_FACE ( 'NONE', ( #227, #5265 ), #169, .F. ) ;
#6030 = DIRECTION ( 'NONE',  ( -1.000000000000000000, -2.478176394252581696E-17, 0.000000000000000000 ) ) ;
#6031 = CARTESIAN_POINT ( 'NONE',  ( -61.99999999999998579, 12.57812499965860198, 2.498450539062049724 ) ) ;
#6032 = DIRECTION ( 'NONE',  ( -0.000000000000000000, -1.000000000000000000, -0.000000000000000000 ) ) ;
#6033 = CARTESIAN_POINT ( 'NONE',  ( -60.99999999999998579, 9.197916665983870033, 2.077350269189628840 ) ) ;
#6034 = ORIENTED_EDGE ( 'NONE', *, *, #10656, .F. ) ;
#6035 = CARTESIAN_POINT ( 'NONE',  ( -61.99999999999998579, 13.56249999999999822, 0.5000000000000013323 ) ) ;
#6036 = ORIENTED_EDGE ( 'NONE', *, *, #6612, .T. ) ;
#6037 = FACE_OUTER_BOUND ( 'NONE', #370, .T. ) ;
#6038 = CARTESIAN_POINT ( 'NONE',  ( -61.99999999999998579, 11.76562499965860198, 2.498450539062049724 ) ) ;
#6039 = EDGE_CURVE ( 'NONE', #2937, #8468, #4550, .T. ) ;
#6040 = ORIENTED_EDGE ( 'NONE', *, *, #7388, .F. ) ;
#6041 = CARTESIAN_POINT ( 'NONE',  ( -62.43234176562498305, 8.723958332991934128, 0.7511620957034662593 ) ) ;
#6042 = CARTESIAN_POINT ( 'NONE',  ( -61.99999999999998579, 10.40624999931720218, 2.500000000000002665 ) ) ;
#6043 = CARTESIAN_POINT ( 'NONE',  ( -61.56765823437498142, 13.43229166632526805, 0.7511620957034663704 ) ) ;
#6044 = LINE ( 'NONE', #2494, #591 ) ;
#6045 = ORIENTED_EDGE ( 'NONE', *, *, #10296, .F. ) ;
#6046 = CARTESIAN_POINT ( 'NONE',  ( 1.299999999999999600, 1.000000000000000000, 0.000000000000000000 ) ) ;
#6047 = ORIENTED_EDGE ( 'NONE', *, *, #7371, .F. ) ;
#6048 = CARTESIAN_POINT ( 'NONE',  ( -60.99999999999998579, 13.23958333265053611, 0.9226497308103762673 ) ) ;
#6049 = CARTESIAN_POINT ( 'NONE',  ( -61.99999999999998579, 15.01562499965860198, 2.498450539062049724 ) ) ;
#6050 = DIRECTION ( 'NONE',  ( -0.000000000000000000, -1.000000000000000000, -0.000000000000000000 ) ) ;
#6051 = CARTESIAN_POINT ( 'NONE',  ( -61.99999999999998579, 26.00000000000000355, 1.500000000000002220 ) ) ;
#6052 = EDGE_CURVE ( 'NONE', #424, #6502, #318, .T. ) ;
#6053 = CARTESIAN_POINT ( 'NONE',  ( -105.0000000000000000, -2.500000000000000000, 4.000000000000000000 ) ) ;
#6054 = CARTESIAN_POINT ( 'NONE',  ( -62.86468353124999453, 14.03645833299193413, 1.999225269531025750 ) ) ;
#6055 = CARTESIAN_POINT ( 'NONE',  ( -61.56765823437498852, 9.286458332991935904, 2.248837904296538515 ) ) ;
#6056 = DIRECTION ( 'NONE',  ( 0.000000000000000000, 0.000000000000000000, -1.000000000000000000 ) ) ;
#6057 =( BOUNDED_CURVE ( )  B_SPLINE_CURVE ( 2, ( #10053, #5730, #2500, #4886, #8396, #3282, #1673, #7615, #7560 ),
 .UNSPECIFIED., .F., .T. ) 
 B_SPLINE_CURVE_WITH_KNOTS ( ( 3, 2, 2, 2, 3 ),
 ( 0.4765625000000000000, 0.4791666666666666852, 0.4843750000000000000, 0.4895833333333333148, 0.4921875000000000000 ),
 .UNSPECIFIED. ) 
 CURVE ( )  GEOMETRIC_REPRESENTATION_ITEM ( )  RATIONAL_B_SPLINE_CURVE ( ( 0.9330127018922194093, 0.9330127018922194093, 1.000000000000000000, 0.8660254037844387076, 1.000000000000000000, 0.8660254037844387076, 1.000000000000000000, 0.9330127018922194093, 0.9330127018922194093 ) ) 
 REPRESENTATION_ITEM ( '' )  );
#6058 = DIRECTION ( 'NONE',  ( -1.000000000000000000, 0.000000000000000000, 0.000000000000000000 ) ) ;
#6059 = AXIS2_PLACEMENT_3D ( 'NONE', #171, #3667, #460 ) ;
#6060 = CARTESIAN_POINT ( 'NONE',  ( -61.13531646874998415, 9.619791666325268054, 1.999225269531026417 ) ) ;
#6061 = CARTESIAN_POINT ( 'NONE',  ( -61.49999999999998579, 15.76041666598386826, 0.6339745962155628467 ) ) ;
#6062 = ORIENTED_EDGE ( 'NONE', *, *, #7357, .F. ) ;
#6063 = CARTESIAN_POINT ( 'NONE',  ( -61.99999999999998579, 16.00000000000000000, 0.5000000000000041078 ) ) ;
#6064 = EDGE_CURVE ( 'NONE', #4883, #7434, #2011, .T. ) ;
#6065 = CIRCLE ( 'NONE', #4995, 40.00000000000000711 ) ;
#6066 = CARTESIAN_POINT ( 'NONE',  ( -61.56765823437498142, 15.86979166632526628, 0.7511620957034663704 ) ) ;
#6067 = CARTESIAN_POINT ( 'NONE',  ( -61.13531646874998415, 11.32812499965860020, 1.500000000000002220 ) ) ;
#6068 = CARTESIAN_POINT ( 'NONE',  ( -61.13531646874997705, 9.057291666325266277, 1.999225269531026417 ) ) ;
#6069 = CARTESIAN_POINT ( 'NONE',  ( -76.99999999999998579, 11.49999999999999645, 8.000000000000000000 ) ) ;
#6070 = VERTEX_POINT ( 'NONE', #5385 ) ;
#6071 = CARTESIAN_POINT ( 'NONE',  ( -60.99999999999998579, 15.52083333333333215, 0.9226497308103762673 ) ) ;
#6072 = CARTESIAN_POINT ( 'NONE',  ( -62.86468353124998032, 10.24479166632526628, 1.000774730468978024 ) ) ;
#6073 =( LENGTH_UNIT ( ) NAMED_UNIT ( * ) SI_UNIT ( .MILLI., .METRE. ) );
#6074 = CARTESIAN_POINT ( 'NONE',  ( -60.99999999999998579, 13.69791666598386826, 2.077350269189628840 ) ) ;
#6075 = DIRECTION ( 'NONE',  ( 0.000000000000000000, -3.552713678800500929E-15, 1.000000000000000000 ) ) ;
#6076 = VERTEX_POINT ( 'NONE', #3554 ) ;
#6077 = CIRCLE ( 'NONE', #425, 1.000000000000000888 ) ;
#6078 = AXIS2_PLACEMENT_3D ( 'NONE', #8608, #2604, #2498 ) ;
#6079 = CARTESIAN_POINT ( 'NONE',  ( -61.99999999999998579, 11.68749999999999822, 2.500000000000002665 ) ) ;
#6080 = CARTESIAN_POINT ( 'NONE',  ( -62.86468353124998032, 11.43229166632526805, 1.000774730468978024 ) ) ;
#6081 = ORIENTED_EDGE ( 'NONE', *, *, #9667, .F. ) ;
#6082 = CARTESIAN_POINT ( 'NONE',  ( -60.99999999999998579, 11.75000000000000000, 1.500000000000002220 ) ) ;
#6083 = AXIS2_PLACEMENT_3D ( 'NONE', #4337, #7026, #6190 ) ;
#6084 = EDGE_CURVE ( 'NONE', #5526, #9814, #9329, .T. ) ;
#6085 = DIRECTION ( 'NONE',  ( 0.000000000000000000, -0.000000000000000000, 1.000000000000000000 ) ) ;
#6086 = CARTESIAN_POINT ( 'NONE',  ( -61.13531646874998415, 14.16145833299193413, 1.000774730468978468 ) ) ;
#6087 =( NAMED_UNIT ( * ) SI_UNIT ( $, .STERADIAN. ) SOLID_ANGLE_UNIT ( ) );
#6088 = DIRECTION ( 'NONE',  ( -0.000000000000000000, -0.000000000000000000, -1.000000000000000000 ) ) ;
#6089 = CARTESIAN_POINT ( 'NONE',  ( -62.99999999999998579, 9.072916665983868256, 0.9226497308103756012 ) ) ;
#6090 = EDGE_CURVE ( 'NONE', #9455, #1648, #10441, .T. ) ;
#6091 = VERTEX_POINT ( 'NONE', #2231 ) ;
#6092 = DIRECTION ( 'NONE',  ( 0.000000000000000000, 0.000000000000000000, 1.000000000000000000 ) ) ;
#6093 = CIRCLE ( 'NONE', #2722, 6.000000000000005329 ) ;
#6094 = CARTESIAN_POINT ( 'NONE',  ( -62.49999999999998579, 13.33333333333333215, 0.6339745962155627357 ) ) ;
#6095 = CARTESIAN_POINT ( 'NONE',  ( -62.86468353124998742, 11.22395833299193590, 1.999225269531025972 ) ) ;
#6096 = SURFACE_STYLE_FILL_AREA ( #10368 ) ;
#6097 = ORIENTED_EDGE ( 'NONE', *, *, #6039, .F. ) ;
#6098 = CARTESIAN_POINT ( 'NONE',  ( -61.56765823437498142, 8.932291666325268054, 0.7511620957034663704 ) ) ;
#6099 = CARTESIAN_POINT ( 'NONE',  ( -134.9999999999999147, 8.000000000000000000, 3.000000000000000000 ) ) ;
#6100 = CARTESIAN_POINT ( 'NONE',  ( -62.43234176562499016, 14.05729166632526805, 2.248837904296538071 ) ) ;
#6101 = CARTESIAN_POINT ( 'NONE',  ( -62.99999999999998579, 12.09374999931720218, 1.500000000000001998 ) ) ;
#6102 = VERTEX_POINT ( 'NONE', #9005 ) ;
#6103 = CARTESIAN_POINT ( 'NONE',  ( -61.99999999999998579, 12.90624999931720218, 2.500000000000002665 ) ) ;
#6104 = EDGE_CURVE ( 'NONE', #9827, #5253, #3653, .T. ) ;
#6105 = ORIENTED_EDGE ( 'NONE', *, *, #9859, .T. ) ;
#6106 = CARTESIAN_POINT ( 'NONE',  ( -105.0000000000000000, 0.000000000000000000, 3.000000000000000000 ) ) ;
#6107 = CARTESIAN_POINT ( 'NONE',  ( -61.49999999999998579, 8.708333333333333925, 2.366025403784441927 ) ) ;
#6108 = DIRECTION ( 'NONE',  ( -1.000000000000000000, 0.000000000000000000, 0.000000000000000000 ) ) ;
#6109 = CARTESIAN_POINT ( 'NONE',  ( -61.49999999999998579, 12.54166666666666607, 0.6339745962155628467 ) ) ;
#6110 = DIRECTION ( 'NONE',  ( 0.000000000000000000, 0.000000000000000000, -1.000000000000000000 ) ) ;
#6111 = CARTESIAN_POINT ( 'NONE',  ( -62.43234176562498305, 13.47395833299193413, 0.7511620957034662593 ) ) ;
#6112 = CARTESIAN_POINT ( 'NONE',  ( -62.86468353124998032, 8.182291666325269830, 1.000774730468978246 ) ) ;
#6113 = CARTESIAN_POINT ( 'NONE',  ( -61.99999999999998579, 16.00000000000000000, 0.5000000000000041078 ) ) ;
#6114 = DIRECTION ( 'NONE',  ( 0.000000000000000000, -1.000000000000000000, 0.000000000000000000 ) ) ;
#6115 = CARTESIAN_POINT ( 'NONE',  ( -61.13531646874998415, 11.11979166632526805, 1.999225269531026417 ) ) ;
#6116 = DIRECTION ( 'NONE',  ( -0.000000000000000000, -1.000000000000000000, -0.000000000000000000 ) ) ;
#6117 = ORIENTED_EDGE ( 'NONE', *, *, #5750, .T. ) ;
#6118 = PLANE ( 'NONE',  #1238 ) ;
#6119 = CARTESIAN_POINT ( 'NONE',  ( -61.99999999999998579, 12.68750000000000000, 2.500000000000002665 ) ) ;
#6120 = CARTESIAN_POINT ( 'NONE',  ( -61.56765823437498142, 15.36979166632526805, 0.7511620957034663704 ) ) ;
#6121 = CARTESIAN_POINT ( 'NONE',  ( -61.56765823437498142, 12.86979166632526805, 0.7511620957034663704 ) ) ;
#6122 = CARTESIAN_POINT ( 'NONE',  ( -61.56765823437498852, 9.036458332991935904, 2.248837904296538515 ) ) ;
#6123 = FACE_OUTER_BOUND ( 'NONE', #712, .T. ) ;
#6124 =( BOUNDED_CURVE ( )  B_SPLINE_CURVE ( 2, ( #849, #10026, #4230, #2467, #3348, #6751, #800, #73, #3456, #7530, #7578, #5799, #9250, #10911, #8578, #900, #9403, #9348, #3398, #10960, #2628, #4178, #21, #5066, #6806, #10122, #6016, #10178, #4134, #1797, #8464, #6855, #2521, #5911, #4964, #5168, #1637, #5015, #8417, #3300, #5960, #10071, #4282, #9301, #8520, #1691, #9198, #5855, #2574, #1742, #5115, #7691, #750, #10859, #4079, #3247, #7480, #6651, #2409, #1580, #8365, #7857, #10458, #4455, #7972, #7746, #6965, #6305, #240, #7802, #10399, #5452, #124, #10346, #5397, #8748, #3511, #6247, #3625, #1186, #5336, #2743, #2860, #1068, #1966, #5278, #6185, #1129, #4511, #4564, #7914, #8804, #10283, #6914, #185, #1907, #4390, #1856, #2688, #1008, #6129, #6072, #2917, #9632, #9457, #355, #9513, #5224, #2026, #294, #7077, #8630, #8687, #2797, #3565, #3742, #7139, #7020, #9573, #10520, #3677, #9687, #2080, #955, #4334, #1364, #10575, #3028, #1307, #7193, #7406, #4790, #4731, #6420, #4011, #2971, #529, #3178, #3804, #1413, #10788, #3857, #2296, #5625, #419, #3129, #8141, #9075, #2246, #9803, #10743, #472, #3913, #10689, #1466, #8195, #8972, #3966, #9020, #6526, #5516, #4627, #8090, #2197, #4683, #9744, #6357, #8919, #7246, #10628, #581, #9908, #8029, #2344, #2141, #6584, #5575, #7304, #5682, #3079, #6477, #9858, #7355, #4840, #8248, #632, #9963, #8860, #1247, #3383, #6788, #5733, #1562, #10895, #7512, #5837, #9234, #7463, #7674, #1514, #10160, #3285, #886, #4061, #8399, #56, #676, #10209, #2557, #3440, #3, #5048, #1618, #4265, #4162, #8349, #10940, #1723, #10841, #783, #6680, #5782, #6838, #6733, #5098, #2444, #7563, #6633, #9127, #10056, #4996, #3329, #4945, #7618, #8448, #8503, #832, #4889, #10107, #4213, #732, #8291, #5944, #9331, #3226, #10010, #2392, #9284, #1676, #2503, #9176, #4115, #5892, #166, #9496, #1113, #6111, #9612, #9386, #8613, #7953, #7784, #8559, #5153, #7899, #1891, #2844, #7006, #3551, #4494, #5210, #5262, #4437, #6231, #9555, #2728, #8729, #10384, #277, #10266, #1781, #1839, #6948, #6054, #3492, #940, #2674, #992, #9441, #1949, #3662, #4319, #7121, #7729, #335, #4372, #10327, #7058, #108, #8667, #3723, #1049, #10439, #2007, #7838, #223, #5381, #3609, #8787, #1168, #2609, #2780, #6167, #5318, #4547, #5997, #6894, #3785, #10501, #397, #4609, #2900, #9672, #1228, #6287, #2063, #5436, #8841, #8012, #4226, #9297, #5851, #5110, #8413, #1575, #4174, #5956, #691, #5011, #4130, #5745, #896, #10955, #9344, #6692, #796, #10855, #4277, #7526, #10907, #3296, #9192, #845, #1687, #1737, #5062, #8516, #7574, #8460, #4960, #7686, #8361, #2517, #2570, #6647, #9139, #7631, #1528, #5907, #69, #3343, #9975, #5795, #6802, #3452, #6746, #10118, #3394, #3242, #16, #10174, #746, #2357, #4902, #8302 ),
 .UNSPECIFIED., .F., .T. ) 
 B_SPLINE_CURVE_WITH_KNOTS ( ( 3, 2, 2, 2, 2, 2, 2, 2, 2, 2, 2, 2, 2, 2, 2, 2, 2, 2, 2, 2, 2, 2, 2, 2, 2, 2, 2, 2, 2, 2, 2, 2, 2, 2, 2, 2, 2, 2, 2, 2, 2, 2, 2, 2, 2, 2, 2, 2, 2, 2, 2, 2, 2, 2, 2, 2, 2, 2, 2, 2, 2, 2, 2, 2, 2, 2, 2, 2, 2, 2, 2, 2, 2, 2, 2, 2, 2, 2, 2, 2, 2, 2, 2, 2, 2, 2, 2, 2, 2, 2, 2, 2, 2, 2, 2, 2, 2, 2, 2, 2, 2, 2, 2, 2, 2, 2, 2, 2, 2, 2, 2, 2, 2, 2, 2, 2, 2, 2, 2, 2, 2, 2, 2, 2, 2, 2, 2, 2, 2, 2, 2, 2, 2, 2, 2, 2, 2, 2, 2, 2, 2, 2, 2, 2, 2, 2, 2, 2, 2, 2, 2, 2, 2, 2, 2, 2, 2, 2, 2, 2, 2, 2, 2, 2, 2, 2, 2, 2, 2, 2, 2, 2, 2, 2, 2, 2, 2, 2, 2, 2, 2, 2, 2, 2, 2, 2, 2, 2, 2, 2, 2, 2, 3 ),
 ( 0.000000000000000000, 0.005208333333333333044, 0.01041666666666666609, 0.01562500000000000000, 0.02083333333333333218, 0.02604166666666666782, 0.03125000000000000000, 0.03645833333333333565, 0.04166666666666666435, 0.04687500000000000000, 0.05208333333333333565, 0.05729166666666666435, 0.06250000000000000000, 0.06770833333333332871, 0.07291666666666667129, 0.07812500000000000000, 0.08333333333333332871, 0.08854166666666667129, 0.09375000000000000000, 0.09895833333333332871, 0.1041666666666666713, 0.1093750000000000000, 0.1145833333333333287, 0.1197916666666666713, 0.1250000000000000000, 0.1302083333333333426, 0.1354166666666666574, 0.1406250000000000000, 0.1458333333333333426, 0.1510416666666666574, 0.1562500000000000000, 0.1614583333333333426, 0.1666666666666666574, 0.1718750000000000000, 0.1770833333333333426, 0.1822916666666666574, 0.1875000000000000000, 0.1927083333333333426, 0.1979166666666666574, 0.2031250000000000000, 0.2083333333333333426, 0.2135416666666666574, 0.2187500000000000000, 0.2239583333333333426, 0.2291666666666666574, 0.2343750000000000000, 0.2395833333333333426, 0.2447916666666666574, 0.2500000000000000000, 0.2552083333333333148, 0.2604166666666666852, 0.2656250000000000000, 0.2708333333333333148, 0.2760416666666666852, 0.2812500000000000000, 0.2864583333333333148, 0.2916666666666666852, 0.2968750000000000000, 0.3020833333333333148, 0.3072916666666666852, 0.3125000000000000000, 0.3177083333333333148, 0.3229166666666666852, 0.3281250000000000000, 0.3333333333333333148, 0.3385416666666666852, 0.3437500000000000000, 0.3489583333333333148, 0.3541666666666666852, 0.3593750000000000000, 0.3645833333333333148, 0.3697916666666666852, 0.3750000000000000000, 0.3802083333333333148, 0.3854166666666666852, 0.3906250000000000000, 0.3958333333333333148, 0.4010416666666666852, 0.4062500000000000000, 0.4114583333333333148, 0.4166666666666666852, 0.4218750000000000000, 0.4270833333333333148, 0.4322916666666666852, 0.4375000000000000000, 0.4427083333333333148, 0.4479166666666666852, 0.4531250000000000000, 0.4583333333333333148, 0.4635416666666666852, 0.4687500000000000000, 0.4739583333333333148, 0.4791666666666666852, 0.4843750000000000000, 0.4895833333333333148, 0.4947916666666666852, 0.5000000000000000000, 0.5052083333333333703, 0.5104166666666666297, 0.5156250000000000000, 0.5208333333333333703, 0.5260416666666666297, 0.5312500000000000000, 0.5364583333333333703, 0.5416666666666666297, 0.5468750000000000000, 0.5520833333333333703, 0.5572916666666666297, 0.5625000000000000000, 0.5677083333333333703, 0.5729166666666666297, 0.5781250000000000000, 0.5833333333333333703, 0.5885416666666666297, 0.5937500000000000000, 0.5989583333333333703, 0.6041666666666666297, 0.6093750000000000000, 0.6145833333333333703, 0.6197916666666666297, 0.6250000000000000000, 0.6302083333333333703, 0.6354166666666666297, 0.6406250000000000000, 0.6458333333333333703, 0.6510416666666666297, 0.6562500000000000000, 0.6614583333333333703, 0.6666666666666666297, 0.6718750000000000000, 0.6770833333333333703, 0.6822916666666666297, 0.6875000000000000000, 0.6927083333333333703, 0.6979166666666666297, 0.7031250000000000000, 0.7083333333333333703, 0.7135416666666666297, 0.7187500000000000000, 0.7239583333333333703, 0.7291666666666666297, 0.7343750000000000000, 0.7395833333333333703, 0.7447916666666666297, 0.7500000000000000000, 0.7552083333333333703, 0.7604166666666666297, 0.7656250000000000000, 0.7708333333333333703, 0.7760416666666666297, 0.7812500000000000000, 0.7864583333333333703, 0.7916666666666666297, 0.7968750000000000000, 0.8020833333333333703, 0.8072916666666666297, 0.8125000000000000000, 0.8177083333333333703, 0.8229166666666666297, 0.8281250000000000000, 0.8333333333333333703, 0.8385416666666666297, 0.8437500000000000000, 0.8489583333333333703, 0.8541666666666666297, 0.8593750000000000000, 0.8645833333333333703, 0.8697916666666666297, 0.8750000000000000000, 0.8802083333333333703, 0.8854166666666666297, 0.8906250000000000000, 0.8958333333333333703, 0.9010416666666666297, 0.9062500000000000000, 0.9114583333333333703, 0.9166666666666666297, 0.9218750000000000000, 0.9270833333333333703, 0.9322916666666666297, 0.9375000000000000000, 0.9427083333333333703, 0.9479166666666666297, 0.9531250000000000000, 0.9583333333333333703, 0.9635416666666666297, 0.9687500000000000000, 0.9739583333333333703, 0.9791666666666666297, 0.9843750000000000000, 0.9895833333333333703, 0.9947916666666666297, 1.000000000000000000 ),
 .UNSPECIFIED. ) 
 CURVE ( )  GEOMETRIC_REPRESENTATION_ITEM ( )  RATIONAL_B_SPLINE_CURVE ( ( 1.000000000000000000, 0.8660254037844387076, 1.000000000000000000, 0.8660254037844387076, 1.000000000000000000, 0.8660254037844387076, 1.000000000000000000, 0.8660254037844387076, 1.000000000000000000, 0.8660254037844387076, 1.000000000000000000, 0.8660254037844387076, 1.000000000000000000, 0.8660254037844387076, 1.000000000000000000, 0.8660254037844387076, 1.000000000000000000, 0.8660254037844387076, 1.000000000000000000, 0.8660254037844387076, 1.000000000000000000, 0.8660254037844387076, 1.000000000000000000, 0.8660254037844387076, 1.000000000000000000, 0.8660254037844387076, 1.000000000000000000, 0.8660254037844387076, 1.000000000000000000, 0.8660254037844387076, 1.000000000000000000, 0.8660254037844387076, 1.000000000000000000, 0.8660254037844387076, 1.000000000000000000, 0.8660254037844387076, 1.000000000000000000, 0.8660254037844387076, 1.000000000000000000, 0.8660254037844387076, 1.000000000000000000, 0.8660254037844387076, 1.000000000000000000, 0.8660254037844387076, 1.000000000000000000, 0.8660254037844387076, 1.000000000000000000, 0.8660254037844387076, 1.000000000000000000, 0.8660254037844387076, 1.000000000000000000, 0.8660254037844387076, 1.000000000000000000, 0.8660254037844387076, 1.000000000000000000, 0.8660254037844387076, 1.000000000000000000, 0.8660254037844387076, 1.000000000000000000, 0.8660254037844387076, 1.000000000000000000, 0.8660254037844387076, 1.000000000000000000, 0.8660254037844387076, 1.000000000000000000, 0.8660254037844387076, 1.000000000000000000, 0.8660254037844387076, 1.000000000000000000, 0.8660254037844387076, 1.000000000000000000, 0.8660254037844387076, 1.000000000000000000, 0.8660254037844387076, 1.000000000000000000, 0.8660254037844387076, 1.000000000000000000, 0.8660254037844387076, 1.000000000000000000, 0.8660254037844387076, 1.000000000000000000, 0.8660254037844387076, 1.000000000000000000, 0.8660254037844387076, 1.000000000000000000, 0.8660254037844387076, 1.000000000000000000, 0.8660254037844387076, 1.000000000000000000, 0.8660254037844387076, 1.000000000000000000, 0.8660254037844387076, 1.000000000000000000, 0.8660254037844387076, 1.000000000000000000, 0.8660254037844387076, 1.000000000000000000, 0.8660254037844387076, 1.000000000000000000, 0.8660254037844387076, 1.000000000000000000, 0.8660254037844387076, 1.000000000000000000, 0.8660254037844387076, 1.000000000000000000, 0.8660254037844387076, 1.000000000000000000, 0.8660254037844387076, 1.000000000000000000, 0.8660254037844387076, 1.000000000000000000, 0.8660254037844387076, 1.000000000000000000, 0.8660254037844387076, 1.000000000000000000, 0.8660254037844387076, 1.000000000000000000, 0.8660254037844387076, 1.000000000000000000, 0.8660254037844387076, 1.000000000000000000, 0.8660254037844387076, 1.000000000000000000, 0.8660254037844387076, 1.000000000000000000, 0.8660254037844387076, 1.000000000000000000, 0.8660254037844387076, 1.000000000000000000, 0.8660254037844387076, 1.000000000000000000, 0.8660254037844387076, 1.000000000000000000, 0.8660254037844387076, 1.000000000000000000, 0.8660254037844387076, 1.000000000000000000, 0.8660254037844387076, 1.000000000000000000, 0.8660254037844387076, 1.000000000000000000, 0.8660254037844387076, 1.000000000000000000, 0.8660254037844387076, 1.000000000000000000, 0.8660254037844387076, 1.000000000000000000, 0.8660254037844387076, 1.000000000000000000, 0.8660254037844387076, 1.000000000000000000, 0.8660254037844387076, 1.000000000000000000, 0.8660254037844387076, 1.000000000000000000, 0.8660254037844387076, 1.000000000000000000, 0.8660254037844387076, 1.000000000000000000, 0.8660254037844387076, 1.000000000000000000, 0.8660254037844387076, 1.000000000000000000, 0.8660254037844387076, 1.000000000000000000, 0.8660254037844387076, 1.000000000000000000, 0.8660254037844387076, 1.000000000000000000, 0.8660254037844387076, 1.000000000000000000, 0.8660254037844387076, 1.000000000000000000, 0.8660254037844387076, 1.000000000000000000, 0.8660254037844387076, 1.000000000000000000, 0.8660254037844387076, 1.000000000000000000, 0.8660254037844387076, 1.000000000000000000, 0.8660254037844387076, 1.000000000000000000, 0.8660254037844387076, 1.000000000000000000, 0.8660254037844387076, 1.000000000000000000, 0.8660254037844387076, 1.000000000000000000, 0.8660254037844387076, 1.000000000000000000, 0.8660254037844387076, 1.000000000000000000, 0.8660254037844387076, 1.000000000000000000, 0.8660254037844387076, 1.000000000000000000, 0.8660254037844387076, 1.000000000000000000, 0.8660254037844387076, 1.000000000000000000, 0.8660254037844387076, 1.000000000000000000, 0.8660254037844387076, 1.000000000000000000, 0.8660254037844387076, 1.000000000000000000, 0.8660254037844387076, 1.000000000000000000, 0.8660254037844387076, 1.000000000000000000, 0.8660254037844387076, 1.000000000000000000, 0.8660254037844387076, 1.000000000000000000, 0.8660254037844387076, 1.000000000000000000, 0.8660254037844387076, 1.000000000000000000, 0.8660254037844387076, 1.000000000000000000, 0.8660254037844387076, 1.000000000000000000, 0.8660254037844387076, 1.000000000000000000, 0.8660254037844387076, 1.000000000000000000, 0.8660254037844387076, 1.000000000000000000, 0.8660254037844387076, 1.000000000000000000, 0.8660254037844387076, 1.000000000000000000, 0.8660254037844387076, 1.000000000000000000, 0.8660254037844387076, 1.000000000000000000, 0.8660254037844387076, 1.000000000000000000, 0.8660254037844387076, 1.000000000000000000, 0.8660254037844387076, 1.000000000000000000, 0.8660254037844387076, 1.000000000000000000, 0.8660254037844387076, 1.000000000000000000, 0.8660254037844387076, 1.000000000000000000, 0.8660254037844387076, 1.000000000000000000, 0.8660254037844387076, 1.000000000000000000, 0.8660254037844387076, 1.000000000000000000, 0.8660254037844387076, 1.000000000000000000, 0.8660254037844387076, 1.000000000000000000, 0.8660254037844387076, 1.000000000000000000, 0.8660254037844387076, 1.000000000000000000, 0.8660254037844387076, 1.000000000000000000, 0.8660254037844387076, 1.000000000000000000, 0.8660254037844387076, 1.000000000000000000, 0.8660254037844387076, 1.000000000000000000, 0.8660254037844387076, 1.000000000000000000, 0.8660254037844387076, 1.000000000000000000, 0.8660254037844387076, 1.000000000000000000, 0.8660254037844387076, 1.000000000000000000, 0.8660254037844387076, 1.000000000000000000, 0.8660254037844387076, 1.000000000000000000, 0.8660254037844387076, 1.000000000000000000, 0.8660254037844387076, 1.000000000000000000, 0.8660254037844387076, 1.000000000000000000, 0.8660254037844387076, 1.000000000000000000, 0.8660254037844387076, 1.000000000000000000, 0.8660254037844387076, 1.000000000000000000, 0.8660254037844387076, 1.000000000000000000, 0.8660254037844387076, 1.000000000000000000, 0.8660254037844387076, 1.000000000000000000, 0.8660254037844387076, 1.000000000000000000, 0.8660254037844387076, 1.000000000000000000, 0.8660254037844387076, 1.000000000000000000, 0.8660254037844387076, 1.000000000000000000, 0.8660254037844387076, 1.000000000000000000, 0.8660254037844387076, 1.000000000000000000, 0.8660254037844387076, 1.000000000000000000, 0.8660254037844387076, 1.000000000000000000, 0.8660254037844387076, 1.000000000000000000, 0.8660254037844387076, 1.000000000000000000, 0.8660254037844387076, 1.000000000000000000, 0.8660254037844387076, 1.000000000000000000, 0.8660254037844387076, 1.000000000000000000, 0.8660254037844387076, 1.000000000000000000, 0.8660254037844387076, 1.000000000000000000, 0.8660254037844387076, 1.000000000000000000, 0.8660254037844387076, 1.000000000000000000, 0.8660254037844387076, 1.000000000000000000, 0.8660254037844387076, 1.000000000000000000, 0.8660254037844387076, 1.000000000000000000, 0.8660254037844387076, 1.000000000000000000, 0.8660254037844387076, 1.000000000000000000, 0.8660254037844387076, 1.000000000000000000, 0.8660254037844387076, 1.000000000000000000, 0.8660254037844387076, 1.000000000000000000, 0.8660254037844387076, 1.000000000000000000, 0.8660254037844387076, 1.000000000000000000, 0.8660254037844387076, 1.000000000000000000, 0.8660254037844387076, 1.000000000000000000, 0.8660254037844387076, 1.000000000000000000, 0.8660254037844387076, 1.000000000000000000, 0.8660254037844387076, 1.000000000000000000, 0.8660254037844387076, 1.000000000000000000, 0.8660254037844387076, 1.000000000000000000, 0.8660254037844387076, 1.000000000000000000, 0.8660254037844387076, 1.000000000000000000, 0.8660254037844387076, 1.000000000000000000, 0.8660254037844387076, 1.000000000000000000, 0.8660254037844387076, 1.000000000000000000, 0.8660254037844387076, 1.000000000000000000, 0.8660254037844387076, 1.000000000000000000, 0.8660254037844387076, 1.000000000000000000 ) ) 
 REPRESENTATION_ITEM ( '' )  );
#6125 = ORIENTED_EDGE ( 'NONE', *, *, #3494, .F. ) ;
#6126 = CARTESIAN_POINT ( 'NONE',  ( -61.49999999999998579, 15.45833333333333393, 2.366025403784441927 ) ) ;
#6127 = ADVANCED_FACE ( 'NONE', ( #5501 ), #9113, .T. ) ;
#6128 = EDGE_CURVE ( 'NONE', #2721, #2734, #1350, .T. ) ;
#6129 = CARTESIAN_POINT ( 'NONE',  ( -62.43234176562498305, 10.22395833299193413, 0.7511620957034662593 ) ) ;
#6130 = FILL_AREA_STYLE_COLOUR ( '', #1591 ) ;
#6131 = CARTESIAN_POINT ( 'NONE',  ( -62.43234176562499016, 15.49479166632526628, 2.248837904296538071 ) ) ;
#6132 = CARTESIAN_POINT ( 'NONE',  ( -60.99999999999998579, 13.44791666598387003, 2.077350269189628840 ) ) ;
#6133 = CARTESIAN_POINT ( 'NONE',  ( 190.0000000000000000, 2.500000000000000000, 4.000000000000000000 ) ) ;
#6134 = EDGE_LOOP ( 'NONE', ( #10605, #1472, #3832, #6703 ) ) ;
#6135 = DIRECTION ( 'NONE',  ( -1.000000000000000000, 1.792547591842700533E-15, 0.000000000000000000 ) ) ;
#6136 = CARTESIAN_POINT ( 'NONE',  ( -62.43234176562498305, 11.66145833299193590, 0.7511620957034662593 ) ) ;
#6137 = CARTESIAN_POINT ( 'NONE',  ( -61.99999999999998579, 16.00000000000000000, 1.500000000000002220 ) ) ;
#6138 = CARTESIAN_POINT ( 'NONE',  ( -61.99999999999998579, 16.00000000000000000, 1.500000000000002220 ) ) ;
#6139 = ORIENTED_EDGE ( 'NONE', *, *, #5886, .T. ) ;
#6140 = CARTESIAN_POINT ( 'NONE',  ( -61.49999999999998579, 10.70833333333333393, 2.366025403784441927 ) ) ;
#6141 = CARTESIAN_POINT ( 'NONE',  ( -61.99999999999998579, 16.00000000000000000, 0.5000000000000041078 ) ) ;
#6142 = CARTESIAN_POINT ( 'NONE',  ( -61.99999999999998579, 13.95312499965860198, 0.5015494609379544944 ) ) ;
#6143 =( NAMED_UNIT ( * ) SI_UNIT ( $, .STERADIAN. ) SOLID_ANGLE_UNIT ( ) );
#6144 = LINE ( 'NONE', #10536, #9930 ) ;
#6145 = CARTESIAN_POINT ( 'NONE',  ( -61.49999999999998579, 9.510416665983870033, 0.6339745962155628467 ) ) ;
#6146 = VERTEX_POINT ( 'NONE', #5611 ) ;
#6147 = DIRECTION ( 'NONE',  ( -0.000000000000000000, 1.000000000000000000, -0.000000000000000000 ) ) ;
#6148 = ADVANCED_FACE ( 'NONE', ( #5561 ), #9951, .T. ) ;
#6149 = CARTESIAN_POINT ( 'NONE',  ( -62.49999999999998579, 15.30208333265053611, 0.6339745962155627357 ) ) ;
#6150 = CARTESIAN_POINT ( 'NONE',  ( -62.86468353124999453, 11.20312499965860020, 1.500000000000002220 ) ) ;
#6151 =( NAMED_UNIT ( * ) SI_UNIT ( $, .STERADIAN. ) SOLID_ANGLE_UNIT ( ) );
#6152 = EDGE_CURVE ( 'NONE', #506, #8992, #524, .T. ) ;
#6153 = ORIENTED_EDGE ( 'NONE', *, *, #697, .T. ) ;
#6154 = CARTESIAN_POINT ( 'NONE',  ( -61.13531646874998415, 10.11979166632526805, 1.999225269531026417 ) ) ;
#6155 = CARTESIAN_POINT ( 'NONE',  ( -120.0000000000000000, -15.00000000000001421, 83.15773105863907233 ) ) ;
#6156 = SHAPE_REPRESENTATION ( 'clamp screw', ( #2307 ), #9766 ) ;
#6157 = CARTESIAN_POINT ( 'NONE',  ( -61.56765823437498852, 14.84895833299193413, 2.248837904296538515 ) ) ;
#6158 = DIRECTION ( 'NONE',  ( 0.000000000000000000, -0.000000000000000000, 1.000000000000000000 ) ) ;
#6159 = ORIENTED_EDGE ( 'NONE', *, *, #2324, .F. ) ;
#6160 = CARTESIAN_POINT ( 'NONE',  ( 0.2309054577385447060, -0.2499999999999997780, -1.812959136724909159 ) ) ;
#6161 = EDGE_LOOP ( 'NONE', ( #4694, #8313, #9571, #6764 ) ) ;
#6162 = CARTESIAN_POINT ( 'NONE',  ( -61.99999999999998579, 12.78124999931720218, 0.5000000000000013323 ) ) ;
#6163 = CARTESIAN_POINT ( 'NONE',  ( -61.99999999999998579, 16.01562499965860198, 2.498450539062049724 ) ) ;
#6164 = DIRECTION ( 'NONE',  ( -0.000000000000000000, -0.000000000000000000, -1.000000000000000000 ) ) ;
#6165 = CARTESIAN_POINT ( 'NONE',  ( -76.89999999999997726, -11.50000000000000711, 4.999999999999999112 ) ) ;
#6166 = CARTESIAN_POINT ( 'NONE',  ( -62.99999999999998579, 8.895833333333333925, 2.077350269189627952 ) ) ;
#6167 = CARTESIAN_POINT ( 'NONE',  ( -61.13531646874998415, 14.64062499965860020, 1.500000000000002220 ) ) ;
#6168 = EDGE_CURVE ( 'NONE', #9700, #3864, #3842, .T. ) ;
#6169 = CARTESIAN_POINT ( 'NONE',  ( -62.86468353124998742, 9.473958332991934128, 1.999225269531025972 ) ) ;
#6170 = CARTESIAN_POINT ( 'NONE',  ( -51.99999999999999289, 3.184081677783117796E-15, 13.00000000000000178 ) ) ;
#6171 = CARTESIAN_POINT ( 'NONE',  ( 0.5000000000000000000, 0.000000000000000000, 0.000000000000000000 ) ) ;
#6172 = VECTOR ( 'NONE', #1513, 1000.000000000000000 ) ;
#6173 = CARTESIAN_POINT ( 'NONE',  ( -61.56765823437498142, 9.932291666325268054, 0.7511620957034663704 ) ) ;
#6174 = CARTESIAN_POINT ( 'NONE',  ( -62.49999999999998579, 14.13541666598387003, 2.366025403784441483 ) ) ;
#6175 = ORIENTED_EDGE ( 'NONE', *, *, #6879, .T. ) ;
#6176 = CARTESIAN_POINT ( 'NONE',  ( 0.5000000000000000000, -0.2499999999999997224, -1.911797424705720116 ) ) ;
#6177 = CARTESIAN_POINT ( 'NONE',  ( -62.49999999999998579, 11.41666666666666785, 2.366025403784441483 ) ) ;
#6178 = CARTESIAN_POINT ( 'NONE',  ( -61.73205080756886076, 9.948664549684629321, 2.500000000000003109 ) ) ;
#6179 = CARTESIAN_POINT ( 'NONE',  ( -62.86468353124999453, 11.95312499965860198, 1.500000000000002220 ) ) ;
#6180 = AXIS2_PLACEMENT_3D ( 'NONE', #4993, #673, #8397 ) ;
#6181 = CARTESIAN_POINT ( 'NONE',  ( -62.86468353124999453, 8.723958332991934128, 1.999225269531025750 ) ) ;
#6182 = CYLINDRICAL_SURFACE ( 'NONE', #10678, 25.99999999999999645 ) ;
#6183 = VERTEX_POINT ( 'NONE', #8280 ) ;
#6184 = CYLINDRICAL_SURFACE ( 'NONE', #1736, 0.9999999999999981126 ) ;
#6185 = CARTESIAN_POINT ( 'NONE',  ( -61.56765823437498142, 9.932291666325268054, 0.7511620957034663704 ) ) ;
#6186 = AXIS2_PLACEMENT_3D ( 'NONE', #6510, #10671, #5557 ) ;
#6187 = DIRECTION ( 'NONE',  ( 0.000000000000000000, 0.000000000000000000, 1.000000000000000000 ) ) ;
#6188 = CARTESIAN_POINT ( 'NONE',  ( -62.86468353124998032, 15.93229166632526805, 1.000774730468978246 ) ) ;
#6189 = CARTESIAN_POINT ( 'NONE',  ( -60.99999999999998579, 14.96874999931720218, 1.500000000000002220 ) ) ;
#6190 = DIRECTION ( 'NONE',  ( -1.000000000000000000, 0.000000000000000000, -0.000000000000000000 ) ) ;
#6191 = ORIENTED_EDGE ( 'NONE', *, *, #8005, .T. ) ;
#6192 = CARTESIAN_POINT ( 'NONE',  ( -105.0000000000000000, -2.500000000000000000, 2.000000000000000000 ) ) ;
#6193 = VECTOR ( 'NONE', #4654, 1000.000000000000000 ) ;
#6194 = CARTESIAN_POINT ( 'NONE',  ( -62.43234176562499016, 11.74479166632526805, 2.248837904296538071 ) ) ;
#6195 = CARTESIAN_POINT ( 'NONE',  ( -62.43234176562499016, 8.494791666325268054, 2.248837904296538071 ) ) ;
#6196 = LINE ( 'NONE', #5176, #8387 ) ;
#6197 = ORIENTED_EDGE ( 'NONE', *, *, #5919, .T. ) ;
#6198 = CARTESIAN_POINT ( 'NONE',  ( -62.99999999999998579, 12.89583333333333037, 2.077350269189627952 ) ) ;
#6199 = CARTESIAN_POINT ( 'NONE',  ( -49.99999999999998579, -2.500000000000000000, 4.000000000000000000 ) ) ;
#6200 = VECTOR ( 'NONE', #5791, 1000.000000000000000 ) ;
#6201 = CARTESIAN_POINT ( 'NONE',  ( -61.56765823437498852, 13.84895833299193413, 2.248837904296538515 ) ) ;
#6202 = ADVANCED_FACE ( 'NONE', ( #10612 ), #5929, .T. ) ;
#6203 = SURFACE_SIDE_STYLE ('',( #10299 ) ) ;
#6204 = DIRECTION ( 'NONE',  ( -0.000000000000000000, -1.000000000000000000, -0.000000000000000000 ) ) ;
#6205 = CARTESIAN_POINT ( 'NONE',  ( -62.99999999999998579, 10.09374999931720218, 1.500000000000001998 ) ) ;
#6206 =( GEOMETRIC_REPRESENTATION_CONTEXT ( 3 ) GLOBAL_UNCERTAINTY_ASSIGNED_CONTEXT ( ( #3847 ) ) GLOBAL_UNIT_ASSIGNED_CONTEXT ( ( #4408, #5129, #6143 ) ) REPRESENTATION_CONTEXT ( 'NONE', 'WORKASPACE' ) );
#6207 = ORIENTED_EDGE ( 'NONE', *, *, #320, .T. ) ;
#6208 = CARTESIAN_POINT ( 'NONE',  ( -61.73205080756886076, 13.55133545031536890, 0.5000000000000014433 ) ) ;
#6209 = APPLICATION_CONTEXT ( 'automotive_design' ) ;
#6210 = CARTESIAN_POINT ( 'NONE',  ( -62.26794919243111082, 13.32366454968462754, 0.5000000000000013323 ) ) ;
#6211 = ADVANCED_FACE ( 'NONE', ( #7279 ), #10662, .F. ) ;
#6212 = VECTOR ( 'NONE', #10679, 1000.000000000000000 ) ;
#6213 = CARTESIAN_POINT ( 'NONE',  ( -62.86468353124998742, 10.72395833299193413, 1.999225269531025972 ) ) ;
#6214 = PRESENTATION_STYLE_ASSIGNMENT (( #10657 ) ) ;
#6215 =( GEOMETRIC_REPRESENTATION_CONTEXT ( 3 ) GLOBAL_UNCERTAINTY_ASSIGNED_CONTEXT ( ( #8067 ) ) GLOBAL_UNIT_ASSIGNED_CONTEXT ( ( #6073, #1010, #2799 ) ) REPRESENTATION_CONTEXT ( 'NONE', 'WORKASPACE' ) );
#6216 = EDGE_LOOP ( 'NONE', ( #6045, #8319, #10087, #9943 ) ) ;
#6217 = CARTESIAN_POINT ( 'NONE',  ( -61.99999999999998579, 9.703124999658601979, 0.5015494609379544944 ) ) ;
#6218 = CARTESIAN_POINT ( 'NONE',  ( 190.0000000000000000, 2.500000000000000000, 2.000000000000000000 ) ) ;
#6219 = VECTOR ( 'NONE', #9210, 1000.000000000000000 ) ;
#6220 = CARTESIAN_POINT ( 'NONE',  ( -61.13531646874998415, 13.91145833299193413, 1.000774730468978468 ) ) ;
#6221 = DIRECTION ( 'NONE',  ( 1.000000000000000000, 0.000000000000000000, 0.000000000000000000 ) ) ;
#6222 = ORIENTED_EDGE ( 'NONE', *, *, #6104, .F. ) ;
#6223 = CARTESIAN_POINT ( 'NONE',  ( -61.99999999999998579, 16.00000000000000000, 2.500000000000000444 ) ) ;
#6224 = VERTEX_POINT ( 'NONE', #4761 ) ;
#6225 = CARTESIAN_POINT ( 'NONE',  ( -61.49999999999998579, 8.791666666666666075, 0.6339745962155628467 ) ) ;
#6226 = CARTESIAN_POINT ( 'NONE',  ( -62.49999999999998579, 8.166666666666667851, 2.366025403784441483 ) ) ;
#6227 = CARTESIAN_POINT ( 'NONE',  ( -77.99999999999998579, 0.000000000000000000, 10.99999999999999289 ) ) ;
#6228 = CARTESIAN_POINT ( 'NONE',  ( -61.99999999999998579, 11.06250000000000000, 0.5000000000000013323 ) ) ;
#6229 = DIRECTION ( 'NONE',  ( -1.000000000000000000, -0.000000000000000000, -0.000000000000000000 ) ) ;
#6230 = EDGE_CURVE ( 'NONE', #7385, #3973, #7329, .T. ) ;
#6231 = CARTESIAN_POINT ( 'NONE',  ( -61.99999999999999289, 13.82812499965860198, 2.498450539062049724 ) ) ;
#6232 = CARTESIAN_POINT ( 'NONE',  ( -61.56765823437498852, 9.536458332991934128, 2.248837904296538515 ) ) ;
#6233 = CARTESIAN_POINT ( 'NONE',  ( -62.49999999999998579, 11.30208333265053611, 0.6339745962155627357 ) ) ;
#6234 = CARTESIAN_POINT ( 'NONE',  ( -61.13531646874998415, 10.89062499965860020, 1.500000000000002220 ) ) ;
#6235 = ADVANCED_FACE ( 'NONE', ( #8223 ), #611, .F. ) ;
#6236 = CARTESIAN_POINT ( 'NONE',  ( -61.99999999999998579, 12.06250000000000000, 0.5000000000000013323 ) ) ;
#6237 = ORIENTED_EDGE ( 'NONE', *, *, #5121, .F. ) ;
#6238 = CARTESIAN_POINT ( 'NONE',  ( 0.04978537780227581394, -0.2499999999999997780, -1.594765474869574540 ) ) ;
#6239 = VERTEX_POINT ( 'NONE', #10721 ) ;
#6240 = CARTESIAN_POINT ( 'NONE',  ( -62.26794919243111082, 10.14508544963257108, 2.500000000000000888 ) ) ;
#6241 = CARTESIAN_POINT ( 'NONE',  ( -61.13531646874998415, 13.05729166632526628, 1.999225269531026417 ) ) ;
#6242 = CARTESIAN_POINT ( 'NONE',  ( -61.99999999999999289, 9.140624999658600203, 0.5015494609379544944 ) ) ;
#6243 = CARTESIAN_POINT ( 'NONE',  ( -62.49999999999998579, 8.583333333333333925, 0.6339745962155627357 ) ) ;
#6244 = ORIENTED_EDGE ( 'NONE', *, *, #6230, .F. ) ;
#6245 = CARTESIAN_POINT ( 'NONE',  ( -62.99999999999998579, 10.82291666598386826, 0.9226497308103756012 ) ) ;
#6246 = AXIS2_PLACEMENT_3D ( 'NONE', #8414, #693, #3979 ) ;
#6247 = CARTESIAN_POINT ( 'NONE',  ( -62.86468353124998032, 9.744791666325268054, 1.000774730468978024 ) ) ;
#6248 = CARTESIAN_POINT ( 'NONE',  ( -77.99999999999998579, 11.49999999999999645, -3.300000000000004263 ) ) ;
#6249 = CARTESIAN_POINT ( 'NONE',  ( -61.13531646874998415, 15.30729166632526983, 1.999225269531026417 ) ) ;
#6250 = CARTESIAN_POINT ( 'NONE',  ( -62.99999999999998579, 14.57291666598387181, 0.9226497308103756012 ) ) ;
#6251 = CARTESIAN_POINT ( 'NONE',  ( -76.89999999999997726, 11.49999999999999645, 4.999999999999999112 ) ) ;
#6252 = ORIENTED_EDGE ( 'NONE', *, *, #4590, .F. ) ;
#6253 = SURFACE_STYLE_FILL_AREA ( #10465 ) ;
#6254 = EDGE_LOOP ( 'NONE', ( #8419, #5373, #3675, #1057 ) ) ;
#6255 = AXIS2_PLACEMENT_3D ( 'NONE', #626, #2386, #10781 ) ;
#6256 = EDGE_CURVE ( 'NONE', #9954, #9681, #6999, .T. ) ;
#6257 = CARTESIAN_POINT ( 'NONE',  ( -61.13531646874997705, 13.05729166632526983, 1.999225269531026417 ) ) ;
#6258 = CARTESIAN_POINT ( 'NONE',  ( -61.99999999999998579, 9.015624999658603755, 2.498450539062049724 ) ) ;
#6259 = LINE ( 'NONE', #7260, #5361 ) ;
#6260 = VERTEX_POINT ( 'NONE', #864 ) ;
#6261 = CARTESIAN_POINT ( 'NONE',  ( -61.99999999999998579, 11.93750000000000000, 2.654700538379254571 ) ) ;
#6262 = DIRECTION ( 'NONE',  ( -1.000000000000000000, -0.000000000000000000, -0.000000000000000000 ) ) ;
#6263 = CARTESIAN_POINT ( 'NONE',  ( -62.86468353124999453, 14.51562499965860020, 1.500000000000002220 ) ) ;
#6264 = AXIS2_PLACEMENT_3D ( 'NONE', #8832, #10600, #8720 ) ;
#6265 = VECTOR ( 'NONE', #3637, 1000.000000000000000 ) ;
#6266 = CARTESIAN_POINT ( 'NONE',  ( -62.99999999999998579, 10.84374999931720218, 1.500000000000001998 ) ) ;
#6267 = ORIENTED_EDGE ( 'NONE', *, *, #10288, .F. ) ;
#6268 = DIRECTION ( 'NONE',  ( -1.000000000000000000, -0.000000000000000000, -0.000000000000000000 ) ) ;
#6269 = EDGE_CURVE ( 'NONE', #386, #9045, #1703, .T. ) ;
#6270 = CARTESIAN_POINT ( 'NONE',  ( -62.43234176562499016, 11.99479166632526628, 2.248837904296538071 ) ) ;
#6271 = EDGE_LOOP ( 'NONE', ( #1039, #4723, #4600, #8149 ) ) ;
#6272 = CARTESIAN_POINT ( 'NONE',  ( -62.86468353124998742, 10.78645833299193413, 1.999225269531025972 ) ) ;
#6273 = DIRECTION ( 'NONE',  ( 1.000000000000000000, 0.000000000000000000, -0.000000000000000000 ) ) ;
#6274 = EDGE_CURVE ( 'NONE', #1452, #1599, #917, .T. ) ;
#6275 = CONICAL_SURFACE ( 'NONE', #50, 1.886264737416298409, 0.08726646259971679309 ) ;
#6276 = CARTESIAN_POINT ( 'NONE',  ( -62.43234176562498305, 14.47395833299193413, 0.7511620957034662593 ) ) ;
#6277 = FACE_OUTER_BOUND ( 'NONE', #10236, .T. ) ;
#6278 = EDGE_LOOP ( 'NONE', ( #7027, #3515, #306, #6377 ) ) ;
#6279 = CARTESIAN_POINT ( 'NONE',  ( -61.99999999999998579, 8.000000000000000000, 1.500000000000002220 ) ) ;
#6280 = VERTEX_POINT ( 'NONE', #10922 ) ;
#6281 = VECTOR ( 'NONE', #4771, 999.9999999999998863 ) ;
#6282 = CARTESIAN_POINT ( 'NONE',  ( -61.73205080756886076, 8.698664549684629321, 2.500000000000003109 ) ) ;
#6283 = CARTESIAN_POINT ( 'NONE',  ( -60.99999999999998579, 8.520833333333333925, 0.9226497308103762673 ) ) ;
#6284 = CARTESIAN_POINT ( 'NONE',  ( 0.000000000000000000, 0.000000000000000000, 3.000000000000000000 ) ) ;
#6285 = CARTESIAN_POINT ( 'NONE',  ( -61.99999999999998579, 14.15624999931720218, 2.500000000000002665 ) ) ;
#6286 = CARTESIAN_POINT ( 'NONE',  ( -61.73205080756888208, 10.66741454900183328, 2.500000000000006661 ) ) ;
#6287 = CARTESIAN_POINT ( 'NONE',  ( -61.13531646874998415, 14.89062499965860020, 1.500000000000002220 ) ) ;
#6288 = CARTESIAN_POINT ( 'NONE',  ( -62.43234176562499016, 10.49479166632526983, 2.248837904296538071 ) ) ;
#6289 = UNCERTAINTY_MEASURE_WITH_UNIT (LENGTH_MEASURE( 1.000000000000000082E-05 ), #4680, 'distance_accuracy_value', 'NONE');
#6290 = CARTESIAN_POINT ( 'NONE',  ( -49.99999999999998579, 3.999999999999980904, -2.000000000000000000 ) ) ;
#6291 = CARTESIAN_POINT ( 'NONE',  ( -62.26794919243111082, 9.676335450315370679, 2.500000000000003109 ) ) ;
#6292 = CARTESIAN_POINT ( 'NONE',  ( -62.86468353124999453, 10.01562499965860198, 1.500000000000002220 ) ) ;
#6293 = CARTESIAN_POINT ( 'NONE',  ( -61.99999999999998579, 8.000000000000000000, 1.500000000000002220 ) ) ;
#6294 = EDGE_LOOP ( 'NONE', ( #6036, #3992 ) ) ;
#6295 = PLANE ( 'NONE',  #2144 ) ;
#6296 = CARTESIAN_POINT ( 'NONE',  ( -0.000000000000000000, -2.500000000000000000, 3.000000000000000000 ) ) ;
#6297 =( BOUNDED_CURVE ( )  B_SPLINE_CURVE ( 2, ( #9757, #4803, #2153, #5525, #369, #5409, #7150, #8929, #8101 ),
 .UNSPECIFIED., .F., .T. ) 
 B_SPLINE_CURVE_WITH_KNOTS ( ( 3, 2, 2, 2, 3 ),
 ( 0.2890624999999999445, 0.2916666666666666852, 0.2968750000000000000, 0.3020833333333333148, 0.3046874999999999445 ),
 .UNSPECIFIED. ) 
 CURVE ( )  GEOMETRIC_REPRESENTATION_ITEM ( )  RATIONAL_B_SPLINE_CURVE ( ( 0.9330127018922192983, 0.9330127018922178550, 1.000000000000000000, 0.8660254037844387076, 1.000000000000000000, 0.8660254037844387076, 1.000000000000000000, 0.9330127018922207416, 0.9330127018922192983 ) ) 
 REPRESENTATION_ITEM ( '' )  );
#6298 = VERTEX_POINT ( 'NONE', #5078 ) ;
#6299 = CARTESIAN_POINT ( 'NONE',  ( -62.49999999999998579, 10.05208333265053611, 0.6339745962155627357 ) ) ;
#6300 = CARTESIAN_POINT ( 'NONE',  ( -61.99999999999998579, 12.39062499965860198, 0.5015494609379544944 ) ) ;
#6301 = EDGE_CURVE ( 'NONE', #5032, #9621, #9374, .T. ) ;
#6302 = CARTESIAN_POINT ( 'NONE',  ( -61.99999999999999289, 10.14062499965860198, 0.5015494609379544944 ) ) ;
#6303 = ORIENTED_EDGE ( 'NONE', *, *, #1166, .F. ) ;
#6304 = CARTESIAN_POINT ( 'NONE',  ( -49.99999999999998579, -18.00000000000001066, 0.000000000000000000 ) ) ;
#6305 = CARTESIAN_POINT ( 'NONE',  ( -62.86468353124999453, 9.536458332991935904, 1.999225269531025750 ) ) ;
#6306 = APPLICATION_PROTOCOL_DEFINITION ( 'draft international standard', 'automotive_design', 1998, #6495 ) ;
#6307 = CARTESIAN_POINT ( 'NONE',  ( -61.13531646874998415, 15.05729166632526805, 1.999225269531026417 ) ) ;
#6308 = CARTESIAN_POINT ( 'NONE',  ( -62.99999999999998579, 14.09374999931720218, 1.500000000000001998 ) ) ;
#6309 = DIRECTION ( 'NONE',  ( 0.000000000000000000, 0.000000000000000000, -1.000000000000000000 ) ) ;
#6310 = ORIENTED_EDGE ( 'NONE', *, *, #3988, .F. ) ;
#6311 = CARTESIAN_POINT ( 'NONE',  ( -61.28647452029539267, 16.00000000000000000, 0.7993707187018740390 ) ) ;
#6312 = ORIENTED_EDGE ( 'NONE', *, *, #9084, .T. ) ;
#6313 = CARTESIAN_POINT ( 'NONE',  ( -62.86468353124998032, 13.18229166632526805, 1.000774730468978024 ) ) ;
#6314 = CARTESIAN_POINT ( 'NONE',  ( -61.13531646874998415, 8.807291666325268054, 1.999225269531026417 ) ) ;
#6315 = CARTESIAN_POINT ( 'NONE',  ( -62.99999999999998579, 8.375000000000000000, 1.500000000000001998 ) ) ;
#6316 = EDGE_LOOP ( 'NONE', ( #5747, #6748, #3647, #10040 ) ) ;
#6317 = CARTESIAN_POINT ( 'NONE',  ( -61.99999999999998579, 12.68750000000000000, 2.654700538379254571 ) ) ;
#6318 = CARTESIAN_POINT ( 'NONE',  ( -49.99998799999998766, -14.00000000000001243, 0.000000000000000000 ) ) ;
#6319 = CARTESIAN_POINT ( 'NONE',  ( -61.13531646874998415, 13.86979166632526805, 1.999225269531026417 ) ) ;
#6320 =( NAMED_UNIT ( * ) PLANE_ANGLE_UNIT ( ) SI_UNIT ( $, .RADIAN. ) );
#6321 = LINE ( 'NONE', #2988, #7268 ) ;
#6322 = EDGE_CURVE ( 'NONE', #1119, #6709, #10136, .T. ) ;
#6323 = CARTESIAN_POINT ( 'NONE',  ( -60.99999999999998579, 10.19791666598387181, 2.077350269189628840 ) ) ;
#6324 = ORIENTED_EDGE ( 'NONE', *, *, #2667, .T. ) ;
#6325 = LINE ( 'NONE', #9708, #3709 ) ;
#6326 = CARTESIAN_POINT ( 'NONE',  ( -62.99999999999998579, 15.34374999931720218, 1.500000000000001998 ) ) ;
#6327 = CARTESIAN_POINT ( 'NONE',  ( -61.99999999999998579, 12.76562499965860198, 2.498450539062049724 ) ) ;
#6328 =( LENGTH_UNIT ( ) NAMED_UNIT ( * ) SI_UNIT ( .MILLI., .METRE. ) );
#6329 = ORIENTED_EDGE ( 'NONE', *, *, #3087, .F. ) ;
#6330 = CARTESIAN_POINT ( 'NONE',  ( -62.86468353124998032, 9.744791666325268054, 1.000774730468978246 ) ) ;
#6331 = DIRECTION ( 'NONE',  ( -1.110223024625156343E-15, -1.000000000000000000, 0.000000000000000000 ) ) ;
#6332 = CARTESIAN_POINT ( 'NONE',  ( -61.13531646874998415, 14.91145833299193413, 1.000774730468978468 ) ) ;
#6333 = CARTESIAN_POINT ( 'NONE',  ( -61.99999999999998579, 16.00000000000000000, 1.500000000000002220 ) ) ;
#6334 = EDGE_LOOP ( 'NONE', ( #4534, #7518, #8866, #10113 ) ) ;
#6335 = FACE_OUTER_BOUND ( 'NONE', #6278, .T. ) ;
#6336 = VERTEX_POINT ( 'NONE', #10192 ) ;
#6337 = CARTESIAN_POINT ( 'NONE',  ( -60.99999999999998579, 12.69791666598386826, 2.077350269189628840 ) ) ;
#6338 = CARTESIAN_POINT ( 'NONE',  ( -60.99999999999998579, 8.500000000000000000, 1.500000000000002220 ) ) ;
#6339 = LINE ( 'NONE', #8071, #8856 ) ;
#6340 = DIRECTION ( 'NONE',  ( 0.000000000000000000, 0.000000000000000000, -1.000000000000000000 ) ) ;
#6341 = CARTESIAN_POINT ( 'NONE',  ( -62.86468353124998032, 10.43229166632526983, 1.000774730468978246 ) ) ;
#6342 = CARTESIAN_POINT ( 'NONE',  ( -61.73205080756886076, 12.02008544963257286, 0.5000000000000014433 ) ) ;
#6343 = CARTESIAN_POINT ( 'NONE',  ( -62.99999999999998579, 9.645833333333330373, 2.077350269189627952 ) ) ;
#6344 = CARTESIAN_POINT ( 'NONE',  ( -61.56765823437498142, 10.43229166632526983, 0.7511620957034663704 ) ) ;
#6345 = CARTESIAN_POINT ( 'NONE',  ( -62.99999999999998579, 13.60416666666666785, 0.9226497308103756012 ) ) ;
#6346 = EDGE_LOOP ( 'NONE', ( #10977, #6470, #3370, #2537 ) ) ;
#6347 = CARTESIAN_POINT ( 'NONE',  ( -134.9999999999999147, 8.000000000000000000, 3.000000000000000000 ) ) ;
#6348 = CARTESIAN_POINT ( 'NONE',  ( -61.99999999999998579, 16.00000000000000000, 1.500000000000002220 ) ) ;
#6349 = AXIS2_PLACEMENT_3D ( 'NONE', #9826, #10485, #10594 ) ;
#6350 = EDGE_CURVE ( 'NONE', #3747, #2994, #5833, .T. ) ;
#6351 = ORIENTED_EDGE ( 'NONE', *, *, #4590, .T. ) ;
#6352 = CARTESIAN_POINT ( 'NONE',  ( -62.43234176562499016, 11.99479166632526628, 2.248837904296538071 ) ) ;
#6353 = CARTESIAN_POINT ( 'NONE',  ( -62.43234176562499016, 9.994791666325268054, 2.248837904296538071 ) ) ;
#6354 = CARTESIAN_POINT ( 'NONE',  ( -61.99999999999998579, 8.562500000000000000, 0.5000000000000013323 ) ) ;
#6355 = ORIENTED_EDGE ( 'NONE', *, *, #9837, .T. ) ;
#6356 = LINE ( 'NONE', #1306, #3877 ) ;
#6357 = CARTESIAN_POINT ( 'NONE',  ( -61.56765823437498852, 11.59895833299193590, 2.248837904296538515 ) ) ;
#6358 = VECTOR ( 'NONE', #8447, 1000.000000000000000 ) ;
#6359 = CARTESIAN_POINT ( 'NONE',  ( -61.99999999999998579, 15.14062499965860198, 0.5015494609379544944 ) ) ;
#6360 = CARTESIAN_POINT ( 'NONE',  ( -60.99999999999998579, 15.23958333265053611, 0.9226497308103762673 ) ) ;
#6361 = EDGE_LOOP ( 'NONE', ( #4925, #5615, #909, #1815 ) ) ;
#6362 = ORIENTED_EDGE ( 'NONE', *, *, #5946, .T. ) ;
#6363 = EDGE_CURVE ( 'NONE', #3475, #10242, #10243, .T. ) ;
#6364 =( BOUNDED_CURVE ( )  B_SPLINE_CURVE ( 2, ( #7609, #4989, #878, #4257, #4204, #3432, #776, #3323, #6723 ),
 .UNSPECIFIED., .F., .T. ) 
 B_SPLINE_CURVE_WITH_KNOTS ( ( 3, 2, 2, 2, 3 ),
 ( 0.3359374999999999445, 0.3385416666666666852, 0.3437500000000000000, 0.3489583333333333148, 0.3515625000000000000 ),
 .UNSPECIFIED. ) 
 CURVE ( )  GEOMETRIC_REPRESENTATION_ITEM ( )  RATIONAL_B_SPLINE_CURVE ( ( 0.9330127018922192983, 0.9330127018922178550, 1.000000000000000000, 0.8660254037844387076, 1.000000000000000000, 0.8660254037844387076, 1.000000000000000000, 0.9330127018922194093, 0.9330127018922194093 ) ) 
 REPRESENTATION_ITEM ( '' )  );
#6365 = CIRCLE ( 'NONE', #1555, 23.99999999999999289 ) ;
#6366 = CARTESIAN_POINT ( 'NONE',  ( -61.99999999999999289, 12.64062499965860198, 0.5015494609379544944 ) ) ;
#6367 = CARTESIAN_POINT ( 'NONE',  ( -61.13531646874998415, 8.348958332991935904, 1.000774730468978468 ) ) ;
#6368 = CIRCLE ( 'NONE', #1029, 1.100000000000003642 ) ;
#6369 = CARTESIAN_POINT ( 'NONE',  ( -61.73205080756886076, 11.80133545031536890, 0.5000000000000014433 ) ) ;
#6370 = EDGE_LOOP ( 'NONE', ( #6777, #5853, #9481, #3325 ) ) ;
#6371 = CARTESIAN_POINT ( 'NONE',  ( -62.99999999999998579, 12.35416666666666785, 0.9226497308103756012 ) ) ;
#6372 = CARTESIAN_POINT ( 'NONE',  ( -62.26794919243110371, 8.645085449632569308, 2.500000000000000888 ) ) ;
#6373 = FACE_OUTER_BOUND ( 'NONE', #6664, .T. ) ;
#6374 = ADVANCED_FACE ( 'NONE', ( #9262 ), #10871, .T. ) ;
#6375 = VECTOR ( 'NONE', #5208, 1000.000000000000000 ) ;
#6376 = CARTESIAN_POINT ( 'NONE',  ( -62.99999999999998579, 10.32291666598387003, 0.9226497308103756012 ) ) ;
#6377 = ORIENTED_EDGE ( 'NONE', *, *, #7333, .F. ) ;
#6378 = EDGE_CURVE ( 'NONE', #8797, #5040, #9311, .T. ) ;
#6379 = VECTOR ( 'NONE', #7178, 1000.000000000000000 ) ;
#6380 = CARTESIAN_POINT ( 'NONE',  ( 0.000000000000000000, 0.000000000000000000, 0.000000000000000000 ) ) ;
#6381 = CARTESIAN_POINT ( 'NONE',  ( -62.86468353124999453, 12.20312499965860198, 1.500000000000002220 ) ) ;
#6382 = ADVANCED_FACE ( 'NONE', ( #4299, #3261, #1540 ), #9155, .T. ) ;
#6383 =( NAMED_UNIT ( * ) SI_UNIT ( $, .STERADIAN. ) SOLID_ANGLE_UNIT ( ) );
#6384 = AXIS2_PLACEMENT_3D ( 'NONE', #2248, #10898, #1622 ) ;
#6385 = VERTEX_POINT ( 'NONE', #5133 ) ;
#6386 =( GEOMETRIC_REPRESENTATION_CONTEXT ( 3 ) GLOBAL_UNCERTAINTY_ASSIGNED_CONTEXT ( ( #8366 ) ) GLOBAL_UNIT_ASSIGNED_CONTEXT ( ( #2040, #4581, #9762 ) ) REPRESENTATION_CONTEXT ( 'NONE', 'WORKASPACE' ) );
#6387 = CARTESIAN_POINT ( 'NONE',  ( -62.43234176562499016, 9.807291666325268054, 2.248837904296538071 ) ) ;
#6388 = CARTESIAN_POINT ( 'NONE',  ( 0.5000000000000000000, 0.2499999999999982792, -2.000000000000000000 ) ) ;
#6389 = CIRCLE ( 'NONE', #3018, 1.000000000000000888 ) ;
#6390 = CARTESIAN_POINT ( 'NONE',  ( -62.86468353124998742, 15.78645833299193590, 1.999225269531025972 ) ) ;
#6391 = PLANE ( 'NONE',  #3768 ) ;
#6392 = ORIENTED_EDGE ( 'NONE', *, *, #445, .F. ) ;
#6393 = FACE_OUTER_BOUND ( 'NONE', #319, .T. ) ;
#6394 = EDGE_CURVE ( 'NONE', #3356, #1702, #6568, .T. ) ;
#6395 = ORIENTED_EDGE ( 'NONE', *, *, #6363, .F. ) ;
#6396 = DIRECTION ( 'NONE',  ( 1.000000000000000000, -0.000000000000000000, -0.000000000000000000 ) ) ;
#6397 = CARTESIAN_POINT ( 'NONE',  ( -61.99999999999998579, 9.812500000000000000, 0.3452994616207497591 ) ) ;
#6398 = CIRCLE ( 'NONE', #1594, 1.099999999999989875 ) ;
#6399 = CARTESIAN_POINT ( 'NONE',  ( -60.99999999999998579, 11.27083333333333393, 0.9226497308103762673 ) ) ;
#6400 = CARTESIAN_POINT ( 'NONE',  ( -61.49999999999998579, 11.95833333333333215, 2.366025403784441927 ) ) ;
#6401 = CARTESIAN_POINT ( 'NONE',  ( -61.99999999999998579, 16.00000000000000000, 1.500000000000002220 ) ) ;
#6402 = CARTESIAN_POINT ( 'NONE',  ( -61.56765823437498852, 10.53645833299193413, 2.248837904296538515 ) ) ;
#6403 = PRODUCT_DEFINITION_FORMATION_WITH_SPECIFIED_SOURCE ( 'ANY', '', #9011, .NOT_KNOWN. ) ;
#6404 = CARTESIAN_POINT ( 'NONE',  ( -61.99999999999998579, 15.90624999931719863, 2.500000000000002665 ) ) ;
#6405 = CARTESIAN_POINT ( 'NONE',  ( -62.86468353124999453, 12.01562499965860198, 1.500000000000002220 ) ) ;
#6406 = FACE_OUTER_BOUND ( 'NONE', #4896, .T. ) ;
#6407 = ORIENTED_EDGE ( 'NONE', *, *, #8312, .F. ) ;
#6408 = EDGE_CURVE ( 'NONE', #10197, #6091, #5974, .T. ) ;
#6409 = FACE_OUTER_BOUND ( 'NONE', #8808, .T. ) ;
#6410 = UNCERTAINTY_MEASURE_WITH_UNIT (LENGTH_MEASURE( 1.000000000000000082E-05 ), #4346, 'distance_accuracy_value', 'NONE');
#6411 = DIRECTION ( 'NONE',  ( -0.000000000000000000, -1.000000000000000000, -0.000000000000000000 ) ) ;
#6412 = EDGE_CURVE ( 'NONE', #2204, #8551, #9208, .T. ) ;
#6413 = ORIENTED_EDGE ( 'NONE', *, *, #3617, .T. ) ;
#6414 = CARTESIAN_POINT ( 'NONE',  ( -61.73205080756886076, 10.27008544963257286, 0.5000000000000014433 ) ) ;
#6415 = CARTESIAN_POINT ( 'NONE',  ( -61.99999999999998579, 14.51562499965860020, 2.498450539062049724 ) ) ;
#6416 = CARTESIAN_POINT ( 'NONE',  ( -61.13531646874997705, 10.80729166632526628, 1.999225269531026417 ) ) ;
#6417 = CARTESIAN_POINT ( 'NONE',  ( -62.99999999999998579, 8.645833333333333925, 2.077350269189627952 ) ) ;
#6418 = ORIENTED_EDGE ( 'NONE', *, *, #10500, .F. ) ;
#6419 = CARTESIAN_POINT ( 'NONE',  ( -61.99999999999998579, 16.00000000000000000, 0.5000000000000041078 ) ) ;
#6420 = CARTESIAN_POINT ( 'NONE',  ( -61.13531646874997705, 10.91145833299193413, 1.000774730468978468 ) ) ;
#6421 = DIRECTION ( 'NONE',  ( 0.000000000000000000, 0.000000000000000000, -1.000000000000000000 ) ) ;
#6422 = CARTESIAN_POINT ( 'NONE',  ( -60.99999999999998579, 16.21874999931720396, 1.500000000000002220 ) ) ;
#6423 = ADVANCED_FACE ( 'NONE', ( #6870 ), #4974, .F. ) ;
#6424 = CARTESIAN_POINT ( 'NONE',  ( -62.49999999999998579, 14.80208333265053611, 0.6339745962155627357 ) ) ;
#6425 = CARTESIAN_POINT ( 'NONE',  ( -61.99999999999998579, 16.00000000000000000, 1.500000000000002220 ) ) ;
#6426 = EDGE_LOOP ( 'NONE', ( #7938, #3773, #9056, #6573 ) ) ;
#6427 = DIRECTION ( 'NONE',  ( -0.000000000000000000, -1.000000000000000000, -0.000000000000000000 ) ) ;
#6428 = ORIENTED_EDGE ( 'NONE', *, *, #2103, .F. ) ;
#6429 = VECTOR ( 'NONE', #9247, 1000.000000000000000 ) ;
#6430 = CARTESIAN_POINT ( 'NONE',  ( -61.13531646874997705, 12.55729166632526805, 1.999225269531026417 ) ) ;
#6431 = CARTESIAN_POINT ( 'NONE',  ( -61.99999999999998579, 9.140624999658601979, 0.5015494609379544944 ) ) ;
#6432 = CARTESIAN_POINT ( 'NONE',  ( -61.99999999999997868, 8.437500000000000000, 2.500000000000002665 ) ) ;
#6433 = VERTEX_POINT ( 'NONE', #8376 ) ;
#6434 = CARTESIAN_POINT ( 'NONE',  ( -62.99999999999998579, 12.37500000000000000, 1.500000000000001998 ) ) ;
#6435 = FACE_OUTER_BOUND ( 'NONE', #7943, .T. ) ;
#6436 = CYLINDRICAL_SURFACE ( 'NONE', #2462, 0.9999999999999981126 ) ;
#6437 = CARTESIAN_POINT ( 'NONE',  ( -61.99999999999998579, 11.03124999931720218, 0.3452994616207497591 ) ) ;
#6438 = ORIENTED_EDGE ( 'NONE', *, *, #3516, .T. ) ;
#6439 =( BOUNDED_CURVE ( )  B_SPLINE_CURVE ( 2, ( #10389, #890, #10165, #9391, #6953, #5158, #6061, #1786, #2679 ),
 .UNSPECIFIED., .F., .F. ) 
 B_SPLINE_CURVE_WITH_KNOTS ( ( 3, 2, 2, 2, 3 ),
 ( 0.9296875000000000000, 0.9322916666666666297, 0.9375000000000000000, 0.9427083333333333703, 0.9453125000000000000 ),
 .UNSPECIFIED. ) 
 CURVE ( )  GEOMETRIC_REPRESENTATION_ITEM ( )  RATIONAL_B_SPLINE_CURVE ( ( 0.9330127018922194093, 0.9330127018922194093, 1.000000000000000000, 0.8660254037844387076, 1.000000000000000000, 0.8660254037844387076, 1.000000000000000000, 0.9330127018922194093, 0.9330127018922194093 ) ) 
 REPRESENTATION_ITEM ( '' )  );
#6440 = ADVANCED_BREP_SHAPE_REPRESENTATION ( '', ( #8688, #2307 ), #9766 ) ;
#6441 = DIRECTION ( 'NONE',  ( 0.000000000000000000, 1.000000000000000000, 0.000000000000000000 ) ) ;
#6442 = CARTESIAN_POINT ( 'NONE',  ( -61.13531646874998415, 12.84895833299193413, 1.000774730468978468 ) ) ;
#6443 = EDGE_CURVE ( 'NONE', #2237, #10334, #5028, .T. ) ;
#6444 = DIRECTION ( 'NONE',  ( 0.000000000000000000, 0.000000000000000000, 1.000000000000000000 ) ) ;
#6445 = ORIENTED_EDGE ( 'NONE', *, *, #8679, .T. ) ;
#6446 = VECTOR ( 'NONE', #4709, 1000.000000000000000 ) ;
#6447 = VECTOR ( 'NONE', #10683, 1000.000000000000000 ) ;
#6448 = ADVANCED_FACE ( 'NONE', ( #4190 ), #9566, .T. ) ;
#6449 = CARTESIAN_POINT ( 'NONE',  ( -62.43234176562498305, 11.22395833299193590, 0.7511620957034662593 ) ) ;
#6450 = DIRECTION ( 'NONE',  ( 1.000000000000000000, 0.000000000000000000, 0.000000000000000000 ) ) ;
#6451 = DIRECTION ( 'NONE',  ( -0.000000000000000000, -0.000000000000000000, 1.000000000000000000 ) ) ;
#6452 = VERTEX_POINT ( 'NONE', #7542 ) ;
#6453 = AXIS2_PLACEMENT_3D ( 'NONE', #9187, #4018, #4222 ) ;
#6454 = CARTESIAN_POINT ( 'NONE',  ( -134.9999999999999147, 10.63932022500203267, 0.000000000000000000 ) ) ;
#6455 = AXIS2_PLACEMENT_3D ( 'NONE', #2696, #7925, #6027 ) ;
#6456 = EDGE_LOOP ( 'NONE', ( #101, #10947, #4297, #2551, #10659, #1019 ) ) ;
#6457 = CARTESIAN_POINT ( 'NONE',  ( -60.99999999999998579, 9.447916665983871809, 2.077350269189628840 ) ) ;
#6458 = CARTESIAN_POINT ( 'NONE',  ( -62.99999999999998579, 10.37500000000000000, 1.500000000000001998 ) ) ;
#6459 = FACE_BOUND ( 'NONE', #4819, .T. ) ;
#6460 = CARTESIAN_POINT ( 'NONE',  ( -60.99999999999998579, 12.22916666666666607, 2.077350269189628840 ) ) ;
#6461 = AXIS2_PLACEMENT_3D ( 'NONE', #7237, #4621, #8020 ) ;
#6462 = CARTESIAN_POINT ( 'NONE',  ( -61.99999999999998579, 8.531249999317203958, 0.3452994616207497591 ) ) ;
#6463 = EDGE_CURVE ( 'NONE', #1648, #9455, #4775, .T. ) ;
#6464 = CARTESIAN_POINT ( 'NONE',  ( -61.13531646874998415, 12.41145833299193413, 1.000774730468978468 ) ) ;
#6465 = CARTESIAN_POINT ( 'NONE',  ( -164.9999999999999147, 10.63932022500206642, 3.000000000000000000 ) ) ;
#6466 = ORIENTED_EDGE ( 'NONE', *, *, #9482, .T. ) ;
#6467 = CARTESIAN_POINT ( 'NONE',  ( -149.9999999999999716, -8.000000000000000000, 0.000000000000000000 ) ) ;
#6468 = CARTESIAN_POINT ( 'NONE',  ( -62.26794919243111082, 9.176335450315367126, 2.500000000000000888 ) ) ;
#6469 = VECTOR ( 'NONE', #8838, 1000.000000000000000 ) ;
#6470 = ORIENTED_EDGE ( 'NONE', *, *, #2021, .T. ) ;
#6471 = CARTESIAN_POINT ( 'NONE',  ( 140.0000000000000284, -2.500000000000000444, 6.000000000000000000 ) ) ;
#6472 = CARTESIAN_POINT ( 'NONE',  ( -61.99999999999998579, 13.89062499965860198, 0.5015494609379544944 ) ) ;
#6473 = CARTESIAN_POINT ( 'NONE',  ( -62.43234176562498305, 9.911458332991934128, 0.7511620957034662593 ) ) ;
#6474 = CARTESIAN_POINT ( 'NONE',  ( -61.49999999999998579, 11.67708333265053611, 2.366025403784441927 ) ) ;
#6475 = ORIENTED_EDGE ( 'NONE', *, *, #6408, .T. ) ;
#6476 = CARTESIAN_POINT ( 'NONE',  ( -77.99999999999998579, -11.50000000000000711, -2.000000000000000000 ) ) ;
#6477 = CARTESIAN_POINT ( 'NONE',  ( -61.13531646874998415, 11.89062499965860198, 1.500000000000002220 ) ) ;
#6478 =( NAMED_UNIT ( * ) SI_UNIT ( $, .STERADIAN. ) SOLID_ANGLE_UNIT ( ) );
#6479 = CARTESIAN_POINT ( 'NONE',  ( -61.99999999999998579, 16.00000000000000000, 2.500000000000000444 ) ) ;
#6480 = CARTESIAN_POINT ( 'NONE',  ( -61.56765823437498852, 8.348958332991934128, 2.248837904296538515 ) ) ;
#6481 = CARTESIAN_POINT ( 'NONE',  ( -164.9999999999999147, 10.63932022500206642, 0.000000000000000000 ) ) ;
#6482 = ORIENTED_EDGE ( 'NONE', *, *, #8531, .F. ) ;
#6483 = CARTESIAN_POINT ( 'NONE',  ( -61.99999999999998579, 15.15624999931720218, 2.500000000000002665 ) ) ;
#6484 = ORIENTED_EDGE ( 'NONE', *, *, #535, .T. ) ;
#6485 = CARTESIAN_POINT ( 'NONE',  ( -62.43234176562498305, 13.16145833299193413, 0.7511620957034662593 ) ) ;
#6486 = EDGE_CURVE ( 'NONE', #10295, #4413, #6778, .T. ) ;
#6487 = CARTESIAN_POINT ( 'NONE',  ( -62.86468353124999453, 9.703124999658601979, 1.500000000000002220 ) ) ;
#6488 = PLANE ( 'NONE',  #1650 ) ;
#6489 = EDGE_LOOP ( 'NONE', ( #10909, #5105, #6902, #159, #9012, #6649, #7489, #7800, #10753, #7884 ) ) ;
#6490 = CARTESIAN_POINT ( 'NONE',  ( -60.99999999999998579, 13.72916666666666785, 2.077350269189628840 ) ) ;
#6491 = LINE ( 'NONE', #4748, #8380 ) ;
#6492 = PRODUCT_DEFINITION_CONTEXT ( 'detailed design', #6209, 'design' ) ;
#6493 = CARTESIAN_POINT ( 'NONE',  ( -60.99999999999998579, 11.69791666598386826, 2.077350269189628840 ) ) ;
#6494 = PLANE ( 'NONE',  #9352 ) ;
#6495 = APPLICATION_CONTEXT ( 'automotive_design' ) ;
#6496 = CARTESIAN_POINT ( 'NONE',  ( -61.13531646874998415, 12.82812499965860198, 1.500000000000002220 ) ) ;
#6497 = ADVANCED_FACE ( 'NONE', ( #2879 ), #3643, .T. ) ;
#6498 = VERTEX_POINT ( 'NONE', #3762 ) ;
#6499 = CARTESIAN_POINT ( 'NONE',  ( -61.99999999999998579, 11.95312499965860198, 0.5015494609379544944 ) ) ;
#6500 = PLANE ( 'NONE',  #2289 ) ;
#6501 = CARTESIAN_POINT ( 'NONE',  ( -62.86468353124998742, 15.28645833299193413, 1.999225269531025972 ) ) ;
#6502 = VERTEX_POINT ( 'NONE', #8594 ) ;
#6503 = DIRECTION ( 'NONE',  ( -1.000000000000000000, 0.000000000000000000, -0.000000000000000000 ) ) ;
#6504 = EDGE_CURVE ( 'NONE', #7831, #1714, #2705, .T. ) ;
#6505 = ORIENTED_EDGE ( 'NONE', *, *, #1848, .T. ) ;
#6506 = CYLINDRICAL_SURFACE ( 'NONE', #10516, 40.00000000000000711 ) ;
#6507 = CARTESIAN_POINT ( 'NONE',  ( -62.99999999999998579, 10.10416666666666785, 0.9226497308103756012 ) ) ;
#6508 = CARTESIAN_POINT ( 'NONE',  ( -57.99999999999998579, -10.00000000000000888, 3.000000000000000000 ) ) ;
#6509 = CARTESIAN_POINT ( 'NONE',  ( -61.99999999999998579, 16.00000000000000000, 1.500000000000002220 ) ) ;
#6510 = CARTESIAN_POINT ( 'NONE',  ( -61.99999999999998579, 16.00000000000000000, 1.500000000000002220 ) ) ;
#6511 = UNCERTAINTY_MEASURE_WITH_UNIT (LENGTH_MEASURE( 1.000000000000000082E-05 ), #10126, 'distance_accuracy_value', 'NONE');
#6512 = CARTESIAN_POINT ( 'NONE',  ( -62.99999999999998579, 15.86458333265053788, 2.077350269189627952 ) ) ;
#6513 = CARTESIAN_POINT ( 'NONE',  ( -62.86468353124998742, 11.53645833299193413, 1.999225269531025972 ) ) ;
#6514 = CARTESIAN_POINT ( 'NONE',  ( -37.99999999999999289, -14.00000000000000888, 5.000000000000000000 ) ) ;
#6515 = EDGE_LOOP ( 'NONE', ( #6125, #1300, #3486, #7185 ) ) ;
#6516 = CARTESIAN_POINT ( 'NONE',  ( -114.9999999999999289, -15.00000000000001421, -2.000000000000000000 ) ) ;
#6517 = DIRECTION ( 'NONE',  ( -0.000000000000000000, -0.000000000000000000, -1.000000000000000000 ) ) ;
#6518 = CARTESIAN_POINT ( 'NONE',  ( -77.99999999999998579, 11.49999999999999645, 5.000000000000000000 ) ) ;
#6519 = FACE_OUTER_BOUND ( 'NONE', #2031, .T. ) ;
#6520 = EDGE_CURVE ( 'NONE', #6385, #7083, #10475, .T. ) ;
#6521 = CARTESIAN_POINT ( 'NONE',  ( -61.13531646874998415, 13.57812499965860198, 1.500000000000002220 ) ) ;
#6522 = CARTESIAN_POINT ( 'NONE',  ( -62.43234176562498305, 10.41145833299193413, 0.7511620957034662593 ) ) ;
#6523 = LINE ( 'NONE', #1410, #7071 ) ;
#6524 = ORIENTED_EDGE ( 'NONE', *, *, #10548, .F. ) ;
#6525 = DIRECTION ( 'NONE',  ( -0.000000000000000000, -1.000000000000000000, -0.000000000000000000 ) ) ;
#6526 = CARTESIAN_POINT ( 'NONE',  ( -61.99999999999999289, 11.45312499965860020, 0.5015494609379544944 ) ) ;
#6527 = CARTESIAN_POINT ( 'NONE',  ( -62.43234176562498305, 14.97395833299193590, 0.7511620957034662593 ) ) ;
#6528 = PRODUCT_DEFINITION ( 'UNKNOWN', '', #1598, #6492 ) ;
#6529 = ITEM_DEFINED_TRANSFORMATION ( 'NONE', 'NONE', #8333,  #2307 ) ;
#6530 = CARTESIAN_POINT ( 'NONE',  ( -62.26794919243111082, 15.17633545031537246, 2.500000000000003109 ) ) ;
#6531 = CARTESIAN_POINT ( 'NONE',  ( -60.99999999999998579, 15.94791666598386826, 2.077350269189628840 ) ) ;
#6532 = DIRECTION ( 'NONE',  ( 0.000000000000000000, 0.000000000000000000, 1.000000000000000000 ) ) ;
#6533 = ORIENTED_EDGE ( 'NONE', *, *, #2667, .F. ) ;
#6534 = CARTESIAN_POINT ( 'NONE',  ( -105.0000000000000000, -2.500000000000000000, 4.000000000000000000 ) ) ;
#6535 = PLANE ( 'NONE',  #10708 ) ;
#6536 = CARTESIAN_POINT ( 'NONE',  ( -61.13531646874998415, 14.32812499965860020, 1.500000000000002220 ) ) ;
#6537 = CARTESIAN_POINT ( 'NONE',  ( -62.43234176562498305, 10.16145833299193413, 0.7511620957034662593 ) ) ;
#6538=STYLED_ITEM('',(#11013),#8521);
#6539 = LINE ( 'NONE', #5796, #8723 ) ;
#6540 = VERTEX_POINT ( 'NONE', #1028 ) ;
#6541 = CARTESIAN_POINT ( 'NONE',  ( -62.49999999999998579, 13.33333333333333215, 0.6339745962155627357 ) ) ;
#6542 = PRODUCT ( 'depth blade', 'depth blade', '', ( #634 ) ) ;
#6543 = CARTESIAN_POINT ( 'NONE',  ( -61.49999999999998579, 8.958333333333333925, 2.366025403784441927 ) ) ;
#6544 = CARTESIAN_POINT ( 'NONE',  ( -61.49999999999998579, 11.76041666598387003, 0.6339745962155628467 ) ) ;
#6545 = EDGE_CURVE ( 'NONE', #5247, #2376, #1872, .T. ) ;
#6546 = CARTESIAN_POINT ( 'NONE',  ( -62.26794919243111082, 14.92633545031537068, 2.500000000000003109 ) ) ;
#6547 = CARTESIAN_POINT ( 'NONE',  ( -61.13531646874998415, 13.34895833299193413, 1.000774730468978468 ) ) ;
#6548 = DIRECTION ( 'NONE',  ( -0.000000000000000000, -1.000000000000000000, -0.000000000000000000 ) ) ;
#6549 = EDGE_CURVE ( 'NONE', #3881, #7921, #9593, .T. ) ;
#6550 = ORIENTED_EDGE ( 'NONE', *, *, #9999, .F. ) ;
#6551 = ADVANCED_BREP_SHAPE_REPRESENTATION ( '', ( #1321, #2307 ), #3714 ) ;
#6552=STYLED_ITEM('',(#11006),#4912);
#6553 = CARTESIAN_POINT ( 'NONE',  ( -61.13531646874998415, 11.89062499965860198, 1.500000000000002220 ) ) ;
#6554 = CARTESIAN_POINT ( 'NONE',  ( -61.49999999999998579, 12.26041666598386826, 0.6339745962155628467 ) ) ;
#6555 = AXIS2_PLACEMENT_3D ( 'NONE', #2380, #9163, #9891 ) ;
#6556 = EDGE_CURVE ( 'NONE', #10524, #2286, #4414, .T. ) ;
#6557 = DIRECTION ( 'NONE',  ( 1.000000000000000000, 0.000000000000000000, 0.000000000000000000 ) ) ;
#6558 = ORIENTED_EDGE ( 'NONE', *, *, #6168, .F. ) ;
#6559 = LINE ( 'NONE', #9105, #7278 ) ;
#6560 = VECTOR ( 'NONE', #1053, 1000.000000000000000 ) ;
#6561 =( BOUNDED_CURVE ( )  B_SPLINE_CURVE ( 2, ( #1189, #3861, #5457, #4631, #9749, #2146, #7143, #8923, #1367 ),
 .UNSPECIFIED., .F., .T. ) 
 B_SPLINE_CURVE_WITH_KNOTS ( ( 3, 2, 2, 2, 3 ),
 ( 0.8046875000000000000, 0.8072916666666666297, 0.8125000000000000000, 0.8177083333333333703, 0.8203125000000000000 ),
 .UNSPECIFIED. ) 
 CURVE ( )  GEOMETRIC_REPRESENTATION_ITEM ( )  RATIONAL_B_SPLINE_CURVE ( ( 0.9330127018922194093, 0.9330127018922194093, 1.000000000000000000, 0.8660254037844387076, 1.000000000000000000, 0.8660254037844387076, 1.000000000000000000, 0.9330127018922194093, 0.9330127018922194093 ) ) 
 REPRESENTATION_ITEM ( '' )  );
#6562 = ORIENTED_EDGE ( 'NONE', *, *, #1550, .F. ) ;
#6563 = FACE_OUTER_BOUND ( 'NONE', #7314, .T. ) ;
#6564 = CARTESIAN_POINT ( 'NONE',  ( -61.99999999999998579, 9.687499999999998224, 2.654700538379254571 ) ) ;
#6565 = DIRECTION ( 'NONE',  ( 0.000000000000000000, 0.000000000000000000, -1.000000000000000000 ) ) ;
#6566 = CARTESIAN_POINT ( 'NONE',  ( -60.99999999999998579, 14.94791666598386826, 2.077350269189628840 ) ) ;
#6567 = CARTESIAN_POINT ( 'NONE',  ( -60.99999999999998579, 12.25000000000000000, 1.500000000000002220 ) ) ;
#6568 = CIRCLE ( 'NONE', #7448, 0.5999999999999999778 ) ;
#6569 = CARTESIAN_POINT ( 'NONE',  ( -62.99999999999998579, 15.82291666598386826, 0.9226497308103756012 ) ) ;
#6570 = CARTESIAN_POINT ( 'NONE',  ( -62.86468353124999453, 12.26562499965860198, 1.500000000000002220 ) ) ;
#6571 = COLOUR_RGB ( '',0.8941176470588234615, 0.8941176470588234615, 0.8941176470588234615 ) ;
#6572 = CARTESIAN_POINT ( 'NONE',  ( -62.49999999999998579, 14.55208333265053611, 0.6339745962155627357 ) ) ;
#6573 = ORIENTED_EDGE ( 'NONE', *, *, #5651, .T. ) ;
#6574 = DIRECTION ( 'NONE',  ( 1.000000000000000000, 0.000000000000000000, 0.000000000000000000 ) ) ;
#6575 = VECTOR ( 'NONE', #1160, 1000.000000000000000 ) ;
#6576 = ORIENTED_EDGE ( 'NONE', *, *, #7371, .T. ) ;
#6577 = LINE ( 'NONE', #5728, #214 ) ;
#6578 = EDGE_CURVE ( 'NONE', #506, #10397, #8711, .T. ) ;
#6579 = CARTESIAN_POINT ( 'NONE',  ( -61.99999999999998579, 13.51562499965860198, 2.498450539062049724 ) ) ;
#6580 = CYLINDRICAL_SURFACE ( 'NONE', #10348, 1.099999999999989875 ) ;
#6581 =( GEOMETRIC_REPRESENTATION_CONTEXT ( 3 ) GLOBAL_UNCERTAINTY_ASSIGNED_CONTEXT ( ( #2363 ) ) GLOBAL_UNIT_ASSIGNED_CONTEXT ( ( #1638, #3349, #2362 ) ) REPRESENTATION_CONTEXT ( 'NONE', 'WORKASPACE' ) );
#6582 = LINE ( 'NONE', #730, #10075 ) ;
#6583 = LINE ( 'NONE', #7354, #8844 ) ;
#6584 = CARTESIAN_POINT ( 'NONE',  ( -62.86468353124999453, 11.78645833299193590, 1.999225269531025750 ) ) ;
#6585 = CARTESIAN_POINT ( 'NONE',  ( -62.86468353124999453, 15.76562499965860198, 1.500000000000002220 ) ) ;
#6586 = EDGE_CURVE ( 'NONE', #4618, #7831, #3531, .T. ) ;
#6587 = LINE ( 'NONE', #6479, #1581 ) ;
#6588 = CARTESIAN_POINT ( 'NONE',  ( -61.49999999999998579, 15.67708333265053611, 2.366025403784441927 ) ) ;
#6589 = CARTESIAN_POINT ( 'NONE',  ( 0.000000000000000000, 0.000000000000000000, 6.000000000000000000 ) ) ;
#6590 = ORIENTED_EDGE ( 'NONE', *, *, #3617, .F. ) ;
#6591 = LINE ( 'NONE', #9082, #867 ) ;
#6592 = DIRECTION ( 'NONE',  ( -0.000000000000000000, -1.000000000000000000, -0.000000000000000000 ) ) ;
#6593 = CARTESIAN_POINT ( 'NONE',  ( -62.86468353124999453, 13.70312499965860198, 1.500000000000002220 ) ) ;
#6594 = CARTESIAN_POINT ( 'NONE',  ( -62.43234176562499016, 10.49479166632526983, 2.248837904296538071 ) ) ;
#6595 = FACE_BOUND ( 'NONE', #973, .T. ) ;
#6596 = ORIENTED_EDGE ( 'NONE', *, *, #9267, .F. ) ;
#6597 = CARTESIAN_POINT ( 'NONE',  ( -62.49999999999998579, 14.16666666666666785, 2.366025403784441483 ) ) ;
#6598 = CARTESIAN_POINT ( 'NONE',  ( -104.9999999999999289, -7.999999999999994671, -2.000000000000000000 ) ) ;
#6599 = SHAPE_REPRESENTATION_RELATIONSHIP ( 'NONE' , 'NONE' ,  #9271, #179 ) ;
#6600 = UNCERTAINTY_MEASURE_WITH_UNIT (LENGTH_MEASURE( 1.000000000000000082E-05 ), #10706, 'distance_accuracy_value', 'NONE');
#6601 = CARTESIAN_POINT ( 'NONE',  ( -60.99999999999998579, 12.46874999931720396, 1.500000000000002220 ) ) ;
#6602 = EDGE_CURVE ( 'NONE', #4626, #6858, #201, .T. ) ;
#6603 = CARTESIAN_POINT ( 'NONE',  ( -61.49999999999998579, 9.541666666666667851, 0.6339745962155628467 ) ) ;
#6604 = CARTESIAN_POINT ( 'NONE',  ( -61.99999999999998579, 14.51562499965860020, 2.498450539062049724 ) ) ;
#6605 = LINE ( 'NONE', #6702, #10232 ) ;
#6606 = ORIENTED_EDGE ( 'NONE', *, *, #6658, .T. ) ;
#6607 = CARTESIAN_POINT ( 'NONE',  ( -61.56765823437498852, 12.09895833299193413, 2.248837904296538515 ) ) ;
#6608 = LINE ( 'NONE', #8112, #4760 ) ;
#6609 = CIRCLE ( 'NONE', #580, 5.000000000000004441 ) ;
#6610 = CARTESIAN_POINT ( 'NONE',  ( -62.86468353124998032, 15.99479166632526805, 1.000774730468978246 ) ) ;
#6611 = ORIENTED_EDGE ( 'NONE', *, *, #6486, .T. ) ;
#6612 = EDGE_CURVE ( 'NONE', #4251, #8110, #5294, .T. ) ;
#6613 = CARTESIAN_POINT ( 'NONE',  ( -62.49999999999998579, 11.08333333333333393, 0.6339745962155627357 ) ) ;
#6614 =( GEOMETRIC_REPRESENTATION_CONTEXT ( 3 ) GLOBAL_UNCERTAINTY_ASSIGNED_CONTEXT ( ( #6511 ) ) GLOBAL_UNIT_ASSIGNED_CONTEXT ( ( #10126, #6811, #701 ) ) REPRESENTATION_CONTEXT ( 'NONE', 'WORKASPACE' ) );
#6615 = ORIENTED_EDGE ( 'NONE', *, *, #479, .F. ) ;
#6616 = CARTESIAN_POINT ( 'NONE',  ( -61.99999999999998579, 9.406249999317202182, 2.500000000000002665 ) ) ;
#6617 = CARTESIAN_POINT ( 'NONE',  ( -60.99999999999998579, 9.979166666666667851, 2.077350269189628840 ) ) ;
#6618 = LINE ( 'NONE', #3063, #2996 ) ;
#6619 = CYLINDRICAL_SURFACE ( 'NONE', #6555, 0.9999999999999981126 ) ;
#6620 = CARTESIAN_POINT ( 'NONE',  ( -60.99999999999998579, 8.239583332650536107, 0.9226497308103762673 ) ) ;
#6621 = CARTESIAN_POINT ( 'NONE',  ( -61.56765823437498852, 11.84895833299193413, 2.248837904296538515 ) ) ;
#6622 = CARTESIAN_POINT ( 'NONE',  ( -62.99999999999998579, 10.60416666666666607, 0.9226497308103756012 ) ) ;
#6623 = ORIENTED_EDGE ( 'NONE', *, *, #657, .T. ) ;
#6624 = CARTESIAN_POINT ( 'NONE',  ( -49.99999999999998579, -4.000000000000019540, -2.000000000000000000 ) ) ;
#6625 = PRODUCT_DEFINITION_SHAPE ( 'NONE', 'NONE',  #10989 ) ;
#6626 = VERTEX_POINT ( 'NONE', #7935 ) ;
#6627 = VECTOR ( 'NONE', #2341, 1000.000000000000000 ) ;
#6628 = CARTESIAN_POINT ( 'NONE',  ( -60.99999999999998579, 13.69791666598387003, 2.077350269189628840 ) ) ;
#6629 = CARTESIAN_POINT ( 'NONE',  ( -61.99999999999998579, 14.01562499965860376, 2.498450539062049724 ) ) ;
#6630 = CARTESIAN_POINT ( 'NONE',  ( 150.0000000000000284, -2.500000000000000000, 3.000000000000000000 ) ) ;
#6631 = CARTESIAN_POINT ( 'NONE',  ( -61.73205080756886076, 11.77008544963257286, 0.5000000000000014433 ) ) ;
#6632 = DIRECTION ( 'NONE',  ( 0.000000000000000000, 0.000000000000000000, 1.000000000000000000 ) ) ;
#6633 = CARTESIAN_POINT ( 'NONE',  ( -61.13531646874997705, 12.86979166632526983, 1.999225269531026417 ) ) ;
#6634 = CARTESIAN_POINT ( 'NONE',  ( -61.56765823437498142, 15.93229166632526628, 0.7511620957034663704 ) ) ;
#6635 = CARTESIAN_POINT ( 'NONE',  ( -61.99999999999998579, 15.06249999999999822, 0.5000000000000013323 ) ) ;
#6636 = SHAPE_DEFINITION_REPRESENTATION ( #5723, #5800 ) ;
#6637 = DIRECTION ( 'NONE',  ( 0.000000000000000000, 0.000000000000000000, -1.000000000000000000 ) ) ;
#6638 = CARTESIAN_POINT ( 'NONE',  ( -60.99999999999998579, 15.96874999931720218, 1.500000000000002220 ) ) ;
#6639 = CARTESIAN_POINT ( 'NONE',  ( -49.99999999999998579, -15.00000000000001243, -2.000000000000000000 ) ) ;
#6640 = ORIENTED_EDGE ( 'NONE', *, *, #5320, .T. ) ;
#6641 = CIRCLE ( 'NONE', #7873, 1.000000000000000888 ) ;
#6642 = DIRECTION ( 'NONE',  ( -0.000000000000000000, -0.000000000000000000, -1.000000000000000000 ) ) ;
#6643 = CARTESIAN_POINT ( 'NONE',  ( -149.9999999999999716, 8.000000000000000000, 3.000000000000000000 ) ) ;
#6644 = ADVANCED_FACE ( 'NONE', ( #7101 ), #5417, .T. ) ;
#6645 = CARTESIAN_POINT ( 'NONE',  ( -61.56765823437498852, 13.78645833299193413, 2.248837904296538515 ) ) ;
#6646 = CARTESIAN_POINT ( 'NONE',  ( -62.43234176562498305, 9.661458332991934128, 0.7511620957034662593 ) ) ;
#6647 = CARTESIAN_POINT ( 'NONE',  ( -62.43234176562498305, 15.72395833299193590, 0.7511620957034662593 ) ) ;
#6648 = FACE_OUTER_BOUND ( 'NONE', #839, .T. ) ;
#6649 = ORIENTED_EDGE ( 'NONE', *, *, #2411, .T. ) ;
#6650 = CARTESIAN_POINT ( 'NONE',  ( -60.99999999999998579, 13.47916666666666785, 2.077350269189628840 ) ) ;
#6651 = CARTESIAN_POINT ( 'NONE',  ( -61.99999999999999289, 9.328124999658600203, 2.498450539062049724 ) ) ;
#6652 = PRESENTATION_STYLE_ASSIGNMENT (( #3248 ) ) ;
#6653 = CARTESIAN_POINT ( 'NONE',  ( -61.49999999999998579, 11.51041666598387003, 0.6339745962155628467 ) ) ;
#6654 = CARTESIAN_POINT ( 'NONE',  ( -61.56765823437498142, 14.61979166632526805, 0.7511620957034663704 ) ) ;
#6655 = CARTESIAN_POINT ( 'NONE',  ( -62.26794919243111082, 15.57366454968462932, 0.5000000000000013323 ) ) ;
#6656 =( BOUNDED_CURVE ( )  B_SPLINE_CURVE ( 2, ( #9193, #747, #797, #3193, #4175, #4903, #10956, #7477, #7368 ),
 .UNSPECIFIED., .F., .T. ) 
 B_SPLINE_CURVE_WITH_KNOTS ( ( 3, 2, 2, 2, 3 ),
 ( 0.7734375000000000000, 0.7760416666666666297, 0.7812500000000000000, 0.7864583333333333703, 0.7890625000000000000 ),
 .UNSPECIFIED. ) 
 CURVE ( )  GEOMETRIC_REPRESENTATION_ITEM ( )  RATIONAL_B_SPLINE_CURVE ( ( 0.9330127018922194093, 0.9330127018922194093, 1.000000000000000000, 0.8660254037844387076, 1.000000000000000000, 0.8660254037844387076, 1.000000000000000000, 0.9330127018922194093, 0.9330127018922194093 ) ) 
 REPRESENTATION_ITEM ( '' )  );
#6657 = ORIENTED_EDGE ( 'NONE', *, *, #2324, .T. ) ;
#6658 = EDGE_CURVE ( 'NONE', #1296, #3152, #7992, .T. ) ;
#6659 = CARTESIAN_POINT ( 'NONE',  ( -61.56765823437498142, 11.43229166632526805, 0.7511620957034663704 ) ) ;
#6660 = CARTESIAN_POINT ( 'NONE',  ( -61.49999999999998579, 11.51041666598387003, 0.6339745962155628467 ) ) ;
#6661 = CARTESIAN_POINT ( 'NONE',  ( 0.6000000000000000888, 1.636698849489768475E-16, -1.336466033005844434 ) ) ;
#6662 = ORIENTED_EDGE ( 'NONE', *, *, #7114, .F. ) ;
#6663 = CARTESIAN_POINT ( 'NONE',  ( -61.73205080756886076, 14.80133545031537068, 0.5000000000000014433 ) ) ;
#6664 = EDGE_LOOP ( 'NONE', ( #1795, #5276, #7904, #5938 ) ) ;
#6665 = DIRECTION ( 'NONE',  ( -0.000000000000000000, -0.000000000000000000, 1.000000000000000000 ) ) ;
#6666 = CARTESIAN_POINT ( 'NONE',  ( -60.99999999999998579, 10.72916666666666607, 2.077350269189628840 ) ) ;
#6667 = DIRECTION ( 'NONE',  ( 0.000000000000000000, 0.000000000000000000, -1.000000000000000000 ) ) ;
#6668 = CARTESIAN_POINT ( 'NONE',  ( -62.26794919243111082, 15.92633545031536890, 2.500000000000003109 ) ) ;
#6669 = CARTESIAN_POINT ( 'NONE',  ( -60.99999999999998579, 8.718749999317203958, 1.500000000000002220 ) ) ;
#6670 = CARTESIAN_POINT ( 'NONE',  ( -62.86468353124999453, 13.01562499965860198, 1.500000000000002220 ) ) ;
#6671 = CARTESIAN_POINT ( 'NONE',  ( -62.99999999999998579, 10.62499999999999822, 1.500000000000001998 ) ) ;
#6672 = ORIENTED_EDGE ( 'NONE', *, *, #6039, .T. ) ;
#6673 = CARTESIAN_POINT ( 'NONE',  ( -77.99999999999998579, 11.49999999999999645, 8.000000000000000000 ) ) ;
#6674 = ORIENTED_EDGE ( 'NONE', *, *, #6602, .F. ) ;
#6675 = DIRECTION ( 'NONE',  ( 1.110223024625156540E-15, 1.000000000000000000, 0.000000000000000000 ) ) ;
#6676 = CARTESIAN_POINT ( 'NONE',  ( -61.56765823437498142, 15.11979166632526805, 0.7511620957034663704 ) ) ;
#6677 = DIRECTION ( 'NONE',  ( 1.000000000000000000, 0.000000000000000000, 0.000000000000000000 ) ) ;
#6678 = SURFACE_SIDE_STYLE ('',( #10938 ) ) ;
#6679 = DIRECTION ( 'NONE',  ( -1.000000000000000000, 0.000000000000000000, 0.000000000000000000 ) ) ;
#6680 = CARTESIAN_POINT ( 'NONE',  ( -62.43234176562498305, 12.72395833299193413, 0.7511620957034662593 ) ) ;
#6681 = CARTESIAN_POINT ( 'NONE',  ( -61.13531646874998415, 16.11979166632526628, 1.999225269531026417 ) ) ;
#6682 = FACE_OUTER_BOUND ( 'NONE', #3598, .T. ) ;
#6683 = DIRECTION ( 'NONE',  ( 0.000000000000000000, 0.000000000000000000, -1.000000000000000000 ) ) ;
#6684 = CARTESIAN_POINT ( 'NONE',  ( -61.99999999999998579, 15.53124999931720218, 0.3452994616207497591 ) ) ;
#6685 = LINE ( 'NONE', #2452, #5881 ) ;
#6686 = VERTEX_POINT ( 'NONE', #7363 ) ;
#6687 = CARTESIAN_POINT ( 'NONE',  ( 11.30000000000000071, 1.000000000000000000, 0.000000000000000000 ) ) ;
#6688 = EDGE_CURVE ( 'NONE', #2680, #8034, #5689, .T. ) ;
#6689 = DIRECTION ( 'NONE',  ( -0.000000000000000000, 1.000000000000000000, -0.000000000000000000 ) ) ;
#6690 = CARTESIAN_POINT ( 'NONE',  ( -61.13531646874997705, 13.80729166632526983, 1.999225269531026417 ) ) ;
#6691 = CARTESIAN_POINT ( 'NONE',  ( -62.43234176562499016, 10.24479166632526805, 2.248837904296538071 ) ) ;
#6692 = CARTESIAN_POINT ( 'NONE',  ( -62.43234176562499016, 15.30729166632526805, 2.248837904296538071 ) ) ;
#6693 = CARTESIAN_POINT ( 'NONE',  ( -105.0000000000000000, -2.500000000000000000, 4.000000000000000000 ) ) ;
#6694 = ORIENTED_EDGE ( 'NONE', *, *, #10652, .T. ) ;
#6695 = CARTESIAN_POINT ( 'NONE',  ( -61.99999999999998579, 13.68750000000000178, 2.654700538379254571 ) ) ;
#6696 = DIRECTION ( 'NONE',  ( 0.000000000000000000, 0.000000000000000000, 1.000000000000000000 ) ) ;
#6697 = UNCERTAINTY_MEASURE_WITH_UNIT (LENGTH_MEASURE( 1.000000000000000082E-05 ), #8208, 'distance_accuracy_value', 'NONE');
#6698 = CARTESIAN_POINT ( 'NONE',  ( -61.99999999999998579, 12.28124999931720396, 0.3452994616207497591 ) ) ;
#6699 = EDGE_CURVE ( 'NONE', #1148, #1253, #4797, .T. ) ;
#6700 = VECTOR ( 'NONE', #2882, 1000.000000000000000 ) ;
#6701 = CARTESIAN_POINT ( 'NONE',  ( -61.13531646874998415, 13.84895833299193413, 1.000774730468978468 ) ) ;
#6702 = CARTESIAN_POINT ( 'NONE',  ( -120.0000000000000000, 3.999999999999980904, -2.000000000000000000 ) ) ;
#6703 = ORIENTED_EDGE ( 'NONE', *, *, #6848, .F. ) ;
#6704 = EDGE_CURVE ( 'NONE', #4361, #2204, #536, .T. ) ;
#6705 = CARTESIAN_POINT ( 'NONE',  ( -61.99999999999998579, 13.45312499965860376, 0.5015494609379544944 ) ) ;
#6706 = PRESENTATION_LAYER_ASSIGNMENT (  '', '', ( #8477 ) ) ;
#6707 = ADVANCED_FACE ( 'NONE', ( #686, #10748, #7471 ), #3233, .F. ) ;
#6708 = DIRECTION ( 'NONE',  ( -1.000000000000000000, 0.000000000000000000, -0.000000000000000000 ) ) ;
#6709 = VERTEX_POINT ( 'NONE', #8200 ) ;
#6710 = CARTESIAN_POINT ( 'NONE',  ( 1.299999999999999156, 1.224646799147353207E-16, -1.000000000000000000 ) ) ;
#6711 = EDGE_CURVE ( 'NONE', #9392, #2994, #9969, .T. ) ;
#6712 =( BOUNDED_CURVE ( )  B_SPLINE_CURVE ( 2, ( #7393, #9890, #1603, #1547, #2229, #768, #662, #3211, #4876 ),
 .UNSPECIFIED., .F., .T. ) 
 B_SPLINE_CURVE_WITH_KNOTS ( ( 3, 2, 2, 2, 3 ),
 ( 0.05468749999999997918, 0.05729166666666666435, 0.06250000000000000000, 0.06770833333333332871, 0.07031249999999995837 ),
 .UNSPECIFIED. ) 
 CURVE ( )  GEOMETRIC_REPRESENTATION_ITEM ( )  RATIONAL_B_SPLINE_CURVE ( ( 0.9330127018922192983, 0.9330127018922187432, 1.000000000000000000, 0.8660254037844387076, 1.000000000000000000, 0.8660254037844387076, 1.000000000000000000, 0.9330127018922204085, 0.9330127018922194093 ) ) 
 REPRESENTATION_ITEM ( '' )  );
#6713 = VERTEX_POINT ( 'NONE', #10018 ) ;
#6714 = CARTESIAN_POINT ( 'NONE',  ( -61.99999999999998579, 11.18749999999999822, 2.654700538379254571 ) ) ;
#6715 = ORIENTED_EDGE ( 'NONE', *, *, #6520, .T. ) ;
#6716 = AXIS2_PLACEMENT_3D ( 'NONE', #2768, #6273, #1992 ) ;
#6717 = CARTESIAN_POINT ( 'NONE',  ( -61.99999999999998579, 8.453124999658601979, 0.5015494609379544944 ) ) ;
#6718 = CARTESIAN_POINT ( 'NONE',  ( -60.99999999999998579, 10.48958333265053611, 0.9226497308103762673 ) ) ;
#6719 = AXIS2_PLACEMENT_3D ( 'NONE', #9861, #8974, #6637 ) ;
#6720 = CARTESIAN_POINT ( 'NONE',  ( -62.43234176562498305, 13.22395833299193413, 0.7511620957034662593 ) ) ;
#6721 = CARTESIAN_POINT ( 'NONE',  ( -62.49999999999998579, 12.88541666598386826, 2.366025403784441483 ) ) ;
#6722 = ORIENTED_EDGE ( 'NONE', *, *, #362, .T. ) ;
#6723 = CARTESIAN_POINT ( 'NONE',  ( -61.99999999999998579, 11.03124999931720218, 0.5000000000000013323 ) ) ;
#6724 = ADVANCED_FACE ( 'NONE', ( #2400 ), #4955, .T. ) ;
#6725 = AXIS2_PLACEMENT_3D ( 'NONE', #3758, #6204, #2815 ) ;
#6726 = EDGE_LOOP ( 'NONE', ( #4681, #33, #2464, #2098 ) ) ;
#6727 = CARTESIAN_POINT ( 'NONE',  ( -61.99999999999998579, 12.81250000000000000, 0.5000000000000013323 ) ) ;
#6728 = CARTESIAN_POINT ( 'NONE',  ( -62.86468353124999453, 15.70312499965860198, 1.500000000000002220 ) ) ;
#6729 = AXIS2_PLACEMENT_3D ( 'NONE', #6763, #1760, #7488 ) ;
#6730 = CARTESIAN_POINT ( 'NONE',  ( -61.99999999999998579, 13.68749999999999822, 2.500000000000002665 ) ) ;
#6731 = CARTESIAN_POINT ( 'NONE',  ( -61.99999999999998579, 8.062500000000000000, 0.5000000000000013323 ) ) ;
#6732 = CARTESIAN_POINT ( 'NONE',  ( 0.5000000000000000000, 0.2499999999999998335, 2.000000000000000000 ) ) ;
#6733 = CARTESIAN_POINT ( 'NONE',  ( -62.86468353124999453, 12.78645833299193413, 1.999225269531025750 ) ) ;
#6734 = CARTESIAN_POINT ( 'NONE',  ( -62.86468353124998742, 15.03645833299193590, 1.999225269531025972 ) ) ;
#6735 = FACE_OUTER_BOUND ( 'NONE', #1682, .T. ) ;
#6736 = CARTESIAN_POINT ( 'NONE',  ( -60.99999999999998579, 13.46874999931720218, 1.500000000000002220 ) ) ;
#6737 = CARTESIAN_POINT ( 'NONE',  ( -62.43234176562499016, 8.807291666325268054, 2.248837904296538071 ) ) ;
#6738 = CARTESIAN_POINT ( 'NONE',  ( -62.49999999999998579, 10.41666666666666785, 2.366025403784441483 ) ) ;
#6739 = ORIENTED_EDGE ( 'NONE', *, *, #7073, .T. ) ;
#6740 = DIRECTION ( 'NONE',  ( -0.000000000000000000, -1.000000000000000000, -0.000000000000000000 ) ) ;
#6741 = CARTESIAN_POINT ( 'NONE',  ( -61.73205080756885366, 8.051335450315370679, 0.5000000000000027756 ) ) ;
#6742 = AXIS2_PLACEMENT_3D ( 'NONE', #9393, #4672, #8081 ) ;
#6743 = ADVANCED_FACE ( 'NONE', ( #790 ), #1419, .T. ) ;
#6744 = CARTESIAN_POINT ( 'NONE',  ( -62.43234176562498305, 15.66145833299193590, 0.7511620957034662593 ) ) ;
#6745 = CARTESIAN_POINT ( 'NONE',  ( -61.56765823437498852, 11.78645833299193413, 2.248837904296538515 ) ) ;
#6746 = CARTESIAN_POINT ( 'NONE',  ( -61.99999999999999289, 15.95312499965860198, 0.5015494609379544944 ) ) ;
#6747 = CARTESIAN_POINT ( 'NONE',  ( -120.0000000000000000, 14.99999999999998579, 0.000000000000000000 ) ) ;
#6748 = ORIENTED_EDGE ( 'NONE', *, *, #3428, .T. ) ;
#6749 = CARTESIAN_POINT ( 'NONE',  ( -60.99999999999998579, 15.25000000000000000, 1.500000000000002220 ) ) ;
#6750 = EDGE_CURVE ( 'NONE', #7755, #8746, #10105, .T. ) ;
#6751 = CARTESIAN_POINT ( 'NONE',  ( -62.86468353124998032, 8.244791666325268054, 1.000774730468978024 ) ) ;
#6752 = VECTOR ( 'NONE', #8171, 1000.000000000000000 ) ;
#6753 = CARTESIAN_POINT ( 'NONE',  ( -62.99999999999998579, 13.61458333265053611, 2.077350269189627952 ) ) ;
#6754 = VERTEX_POINT ( 'NONE', #3186 ) ;
#6755 = DIRECTION ( 'NONE',  ( -0.000000000000000000, -1.000000000000000000, -0.000000000000000000 ) ) ;
#6756 = CARTESIAN_POINT ( 'NONE',  ( -61.99999999999998579, 13.39062499965860020, 0.5015494609379544944 ) ) ;
#6757 = DIRECTION ( 'NONE',  ( 0.000000000000000000, 0.000000000000000000, -1.000000000000000000 ) ) ;
#6758 = ORIENTED_EDGE ( 'NONE', *, *, #2836, .F. ) ;
#6759 = LINE ( 'NONE', #10237, #2921 ) ;
#6760 = CARTESIAN_POINT ( 'NONE',  ( -62.86468353124998032, 12.49479166632526628, 1.000774730468978246 ) ) ;
#6761 = CARTESIAN_POINT ( 'NONE',  ( -61.99999999999998579, 16.00000000000000000, 0.5000000000000041078 ) ) ;
#6762 = ORIENTED_EDGE ( 'NONE', *, *, #2096, .F. ) ;
#6763 = CARTESIAN_POINT ( 'NONE',  ( 145.0000000000000284, -5.500000000000000000, 3.000000000000000000 ) ) ;
#6764 = ORIENTED_EDGE ( 'NONE', *, *, #5250, .F. ) ;
#6765 = CYLINDRICAL_SURFACE ( 'NONE', #1434, 0.9999999999999981126 ) ;
#6766 = EDGE_CURVE ( 'NONE', #7998, #1879, #6591, .T. ) ;
#6767 = EDGE_CURVE ( 'NONE', #6970, #9045, #5845, .T. ) ;
#6768 = ORIENTED_EDGE ( 'NONE', *, *, #6023, .F. ) ;
#6769 = CIRCLE ( 'NONE', #1114, 0.9999999999999983347 ) ;
#6770 = CARTESIAN_POINT ( 'NONE',  ( -61.99999999999998579, 11.68750000000000000, 2.654700538379254571 ) ) ;
#6772 = ORIENTED_EDGE ( 'NONE', *, *, #1644, .T. ) ;
#6771 = APPLICATION_CONTEXT ( 'automotive_design' ) ;
#6773 = CARTESIAN_POINT ( 'NONE',  ( -62.43234176562499016, 9.557291666325268054, 2.248837904296538071 ) ) ;
#6774 = CARTESIAN_POINT ( 'NONE',  ( 0.000000000000000000, 0.2499999999999982792, 1.312875263449799323 ) ) ;
#6775 = CARTESIAN_POINT ( 'NONE',  ( -61.56765823437498142, 12.68229166632526805, 0.7511620957034663704 ) ) ;
#6776 = CARTESIAN_POINT ( 'NONE',  ( -61.99999999999998579, 10.56249999999999822, 0.5000000000000013323 ) ) ;
#6777 = ORIENTED_EDGE ( 'NONE', *, *, #8053, .F. ) ;
#6778 =( BOUNDED_CURVE ( )  B_SPLINE_CURVE ( 2, ( #5187, #9533, #1985, #10481, #10365, #6986, #260, #6208, #6035 ),
 .UNSPECIFIED., .F., .T. ) 
 B_SPLINE_CURVE_WITH_KNOTS ( ( 3, 2, 2, 2, 3 ),
 ( 0.6796875000000000000, 0.6822916666666666297, 0.6875000000000000000, 0.6927083333333333703, 0.6953125000000000000 ),
 .UNSPECIFIED. ) 
 CURVE ( )  GEOMETRIC_REPRESENTATION_ITEM ( )  RATIONAL_B_SPLINE_CURVE ( ( 0.9330127018922194093, 0.9330127018922194093, 1.000000000000000000, 0.8660254037844387076, 1.000000000000000000, 0.8660254037844387076, 1.000000000000000000, 0.9330127018922194093, 0.9330127018922194093 ) ) 
 REPRESENTATION_ITEM ( '' )  );
#6779 = AXIS2_PLACEMENT_3D ( 'NONE', #9132, #8406, #4015 ) ;
#6780 = LINE ( 'NONE', #4155, #7811 ) ;
#6781 = ORIENTED_EDGE ( 'NONE', *, *, #10973, .T. ) ;
#6782 = CARTESIAN_POINT ( 'NONE',  ( -60.99999999999998579, 14.23958333265053611, 0.9226497308103762673 ) ) ;
#6783 = CARTESIAN_POINT ( 'NONE',  ( -62.86468353124998742, 15.47395833299193413, 1.999225269531025972 ) ) ;
#6784 = DIRECTION ( 'NONE',  ( -0.000000000000000000, -0.000000000000000000, -1.000000000000000000 ) ) ;
#6785 = DIRECTION ( 'NONE',  ( -0.000000000000000000, 1.000000000000000000, -0.000000000000000000 ) ) ;
#6786 = CARTESIAN_POINT ( 'NONE',  ( -61.99999999999998579, 8.812500000000000000, 0.5000000000000013323 ) ) ;
#6787 = CONICAL_SURFACE ( 'NONE', #5891, 1.000000000000000888, 1.029744259999999967 ) ;
#6788 = CARTESIAN_POINT ( 'NONE',  ( -61.56765823437498852, 12.09895833299193413, 2.248837904296538515 ) ) ;
#6789 = EDGE_CURVE ( 'NONE', #7083, #8021, #8409, .T. ) ;
#6790 = AXIS2_PLACEMENT_3D ( 'NONE', #2838, #5375, #8782 ) ;
#6791 = CARTESIAN_POINT ( 'NONE',  ( -62.86468353124999453, 8.953124999658601979, 1.500000000000002220 ) ) ;
#6792 = DIRECTION ( 'NONE',  ( -0.000000000000000000, -1.000000000000000000, -0.000000000000000000 ) ) ;
#6793 = CARTESIAN_POINT ( 'NONE',  ( -61.99999999999998579, 13.40624999931720041, 2.500000000000002665 ) ) ;
#6794 = CARTESIAN_POINT ( 'NONE',  ( -61.99999999999998579, 9.703124999658601979, 0.5015494609379544944 ) ) ;
#6795 = EDGE_LOOP ( 'NONE', ( #6562, #7112, #933, #2657 ) ) ;
#6796 = DIRECTION ( 'NONE',  ( -0.000000000000000000, -0.000000000000000000, -1.000000000000000000 ) ) ;
#6797 = LINE ( 'NONE', #6643, #7863 ) ;
#6798 = AXIS2_PLACEMENT_3D ( 'NONE', #687, #9083, #9293 ) ;
#6799 = VECTOR ( 'NONE', #4639, 1000.000000000000000 ) ;
#6800 = CARTESIAN_POINT ( 'NONE',  ( -61.99999999999999289, 15.76562499965860198, 2.498450539062049724 ) ) ;
#6801 = CARTESIAN_POINT ( 'NONE',  ( -62.43234176562498305, 11.41145833299193590, 0.7511620957034662593 ) ) ;
#6802 = CARTESIAN_POINT ( 'NONE',  ( -61.13531646874997705, 15.91145833299193590, 1.000774730468978468 ) ) ;
#6803 = DIRECTION ( 'NONE',  ( -1.000000000000000000, -0.000000000000000000, -0.000000000000000000 ) ) ;
#6804 = ORIENTED_EDGE ( 'NONE', *, *, #1694, .T. ) ;
#6805 = CARTESIAN_POINT ( 'NONE',  ( -60.99999999999998579, 15.47916666666666430, 2.077350269189628840 ) ) ;
#6806 = CARTESIAN_POINT ( 'NONE',  ( -61.13531646874998415, 8.640624999658601979, 1.500000000000002220 ) ) ;
#6807 = VECTOR ( 'NONE', #4284, 1000.000000000000000 ) ;
#6808 = CARTESIAN_POINT ( 'NONE',  ( -61.49999999999998579, 13.26041666598387003, 0.6339745962155628467 ) ) ;
#6809 = PLANE ( 'NONE',  #6083 ) ;
#6810 = VERTEX_POINT ( 'NONE', #2938 ) ;
#6811 =( NAMED_UNIT ( * ) PLANE_ANGLE_UNIT ( ) SI_UNIT ( $, .RADIAN. ) );
#6812 = EDGE_CURVE ( 'NONE', #6713, #10287, #6325, .T. ) ;
#6813 = AXIS2_PLACEMENT_3D ( 'NONE', #4544, #8784, #7950 ) ;
#6814 = CARTESIAN_POINT ( 'NONE',  ( -62.86468353124999453, 11.72395833299193413, 1.999225269531025750 ) ) ;
#6815 = EDGE_LOOP ( 'NONE', ( #5658, #216, #5573, #517, #8607, #10223, #2834, #86 ) ) ;
#6816 = DIRECTION ( 'NONE',  ( -2.478176394252581696E-17, 1.000000000000000000, 0.000000000000000000 ) ) ;
#6817 = CARTESIAN_POINT ( 'NONE',  ( -62.43234176562499016, 13.55729166632526805, 2.248837904296538071 ) ) ;
#6818 = CARTESIAN_POINT ( 'NONE',  ( -61.99999999999998579, 16.00000000000000000, 0.5000000000000041078 ) ) ;
#6819 = EDGE_LOOP ( 'NONE', ( #1488, #157, #8970, #1871 ) ) ;
#6820 = CARTESIAN_POINT ( 'NONE',  ( 145.0000000000000284, -5.500000000000000000, 3.000000000000000888 ) ) ;
#6821 = ORIENTED_EDGE ( 'NONE', *, *, #7194, .T. ) ;
#6822 = FACE_OUTER_BOUND ( 'NONE', #325, .T. ) ;
#6823 = ADVANCED_FACE ( 'NONE', ( #9028 ), #5483, .T. ) ;
#6824 = CARTESIAN_POINT ( 'NONE',  ( -61.13531646874998415, 11.80729166632526805, 1.999225269531026417 ) ) ;
#6825 = ORIENTED_EDGE ( 'NONE', *, *, #771, .T. ) ;
#6826 = CARTESIAN_POINT ( 'NONE',  ( -61.13531646874998415, 8.640624999658601979, 1.500000000000002220 ) ) ;
#6827 = CARTESIAN_POINT ( 'NONE',  ( -62.26794919243111082, 13.89508544963257108, 2.500000000000003109 ) ) ;
#6828 = CARTESIAN_POINT ( 'NONE',  ( -61.56765823437498142, 13.68229166632526805, 0.7511620957034663704 ) ) ;
#6829 = EDGE_CURVE ( 'NONE', #3291, #1599, #2305, .T. ) ;
#6830 = ORIENTED_EDGE ( 'NONE', *, *, #1892, .F. ) ;
#6831 = CARTESIAN_POINT ( 'NONE',  ( -62.26794919243111082, 9.323664549684631098, 0.4999999999999998890 ) ) ;
#6832 = EDGE_LOOP ( 'NONE', ( #775, #2588, #8604, #2276 ) ) ;
#6833 = CARTESIAN_POINT ( 'NONE',  ( -61.99999999999998579, 12.68750000000000000, 2.500000000000002665 ) ) ;
#6834 = CARTESIAN_POINT ( 'NONE',  ( -61.13531646874998415, 14.82812499965860020, 1.500000000000002220 ) ) ;
#6835 = FACE_OUTER_BOUND ( 'NONE', #9420, .T. ) ;
#6836 = CARTESIAN_POINT ( 'NONE',  ( -61.49999999999998579, 12.45833333333333393, 2.366025403784441927 ) ) ;
#6837 = CARTESIAN_POINT ( 'NONE',  ( -62.26794919243111082, 12.39508544963257286, 2.500000000000003109 ) ) ;
#6838 = CARTESIAN_POINT ( 'NONE',  ( -62.86468353124999453, 12.76562499965860198, 1.500000000000002220 ) ) ;
#6839 = CARTESIAN_POINT ( 'NONE',  ( -62.86468353124998742, 8.473958332991934128, 1.999225269531025972 ) ) ;
#6840 = CARTESIAN_POINT ( 'NONE',  ( -61.99999999999998579, 16.00000000000000000, 1.500000000000002220 ) ) ;
#6841 = DIRECTION ( 'NONE',  ( -0.000000000000000000, -0.000000000000000000, -1.000000000000000000 ) ) ;
#6842 = CARTESIAN_POINT ( 'NONE',  ( -62.43234176562499016, 9.807291666325268054, 2.248837904296538071 ) ) ;
#6843 = EDGE_CURVE ( 'NONE', #4689, #10017, #6389, .T. ) ;
#6844 = FACE_OUTER_BOUND ( 'NONE', #8383, .T. ) ;
#6845 = ORIENTED_EDGE ( 'NONE', *, *, #7319, .T. ) ;
#6846 = LINE ( 'NONE', #10168, #10812 ) ;
#6847 = DIRECTION ( 'NONE',  ( 0.000000000000000000, 0.000000000000000000, -1.000000000000000000 ) ) ;
#6848 = EDGE_CURVE ( 'NONE', #9621, #6070, #10114, .T. ) ;
#6849 = CARTESIAN_POINT ( 'NONE',  ( -62.86468353124999453, 15.70312499965860198, 1.500000000000002220 ) ) ;
#6850 = CARTESIAN_POINT ( 'NONE',  ( -62.86468353124998742, 11.22395833299193590, 1.999225269531025972 ) ) ;
#6851 = CARTESIAN_POINT ( 'NONE',  ( -62.43234176562498305, 9.161458332991935904, 0.7511620957034662593 ) ) ;
#6852 = DIRECTION ( 'NONE',  ( 0.000000000000000000, 1.000000000000000000, 0.000000000000000000 ) ) ;
#6853 = ORIENTED_EDGE ( 'NONE', *, *, #7407, .F. ) ;
#6854 = CARTESIAN_POINT ( 'NONE',  ( -61.99999999999998579, 14.68750000000000000, 2.654700538379254571 ) ) ;
#6855 = CARTESIAN_POINT ( 'NONE',  ( -62.86468353124999453, 8.786458332991934128, 1.999225269531025750 ) ) ;
#6856 = CARTESIAN_POINT ( 'NONE',  ( -60.99999999999998579, 13.73958333265053433, 0.9226497308103762673 ) ) ;
#6857 = LINE ( 'NONE', #4393, #3795 ) ;
#6858 = VERTEX_POINT ( 'NONE', #892 ) ;
#6859 = CARTESIAN_POINT ( 'NONE',  ( -61.99999999999998579, 11.56250000000000000, 0.5000000000000013323 ) ) ;
#6860 = CARTESIAN_POINT ( 'NONE',  ( -61.99999999999999289, 11.76562499965860198, 2.498450539062049724 ) ) ;
#6861 = FACE_OUTER_BOUND ( 'NONE', #2616, .T. ) ;
#6862 = CARTESIAN_POINT ( 'NONE',  ( -61.99999999999998579, 16.00000000000000000, 1.500000000000002220 ) ) ;
#6863 = ORIENTED_EDGE ( 'NONE', *, *, #5076, .F. ) ;
#6864 = DIRECTION ( 'NONE',  ( -0.000000000000000000, -0.000000000000000000, 1.000000000000000000 ) ) ;
#6865 = CARTESIAN_POINT ( 'NONE',  ( -62.86468353124999453, 12.51562499965860198, 1.500000000000002220 ) ) ;
#6866 = CARTESIAN_POINT ( 'NONE',  ( -61.99999999999998579, 13.81249999999999822, 0.5000000000000013323 ) ) ;
#6867 = CARTESIAN_POINT ( 'NONE',  ( -61.49999999999998579, 9.260416665983870033, 0.6339745962155628467 ) ) ;
#6868 = EDGE_CURVE ( 'NONE', #6924, #4054, #4380, .T. ) ;
#6869 = ORIENTED_EDGE ( 'NONE', *, *, #2316, .T. ) ;
#6870 = FACE_OUTER_BOUND ( 'NONE', #9774, .T. ) ;
#6871 = VERTEX_POINT ( 'NONE', #65 ) ;
#6872 = CARTESIAN_POINT ( 'NONE',  ( -62.99999999999998579, 12.35416666666666607, 0.9226497308103756012 ) ) ;
#6873 = EDGE_CURVE ( 'NONE', #9265, #470, #5217, .T. ) ;
#6874 = CARTESIAN_POINT ( 'NONE',  ( -62.86468353124998032, 11.43229166632526805, 1.000774730468978246 ) ) ;
#6875 = VERTEX_POINT ( 'NONE', #3391 ) ;
#6876 = CIRCLE ( 'NONE', #3678, 0.9999999999999983347 ) ;
#6877 = CARTESIAN_POINT ( 'NONE',  ( -62.86468353124998032, 8.494791666325268054, 1.000774730468978246 ) ) ;
#6878 = FACE_OUTER_BOUND ( 'NONE', #199, .T. ) ;
#6879 = EDGE_CURVE ( 'NONE', #8912, #211, #9449, .T. ) ;
#6880 = EDGE_CURVE ( 'NONE', #3615, #10979, #1788, .T. ) ;
#6881 = CARTESIAN_POINT ( 'NONE',  ( -61.99999999999998579, 12.95312499965860198, 0.5015494609379544944 ) ) ;
#6882 = CARTESIAN_POINT ( 'NONE',  ( -62.49999999999998579, 12.13541666598386826, 2.366025403784441483 ) ) ;
#6883 = ORIENTED_EDGE ( 'NONE', *, *, #9294, .T. ) ;
#6884 = CARTESIAN_POINT ( 'NONE',  ( -37.99999999999999289, -14.00000000000000888, 5.000000000000000000 ) ) ;
#6885 = AXIS2_PLACEMENT_3D ( 'NONE', #10130, #5071, #28 ) ;
#6886 = PRODUCT_DEFINITION_SHAPE ( 'NONE', 'NONE',  #10988 ) ;
#6887 = CIRCLE ( 'NONE', #10432, 1.336466033005844434 ) ;
#6888 = ORIENTED_EDGE ( 'NONE', *, *, #2354, .T. ) ;
#6889 = CARTESIAN_POINT ( 'NONE',  ( -62.99999999999998579, 10.85416666666666785, 0.9226497308103756012 ) ) ;
#6890 = CARTESIAN_POINT ( 'NONE',  ( -62.43234176562498305, 14.91145833299193590, 0.7511620957034662593 ) ) ;
#6891 = LINE ( 'NONE', #1888, #9460 ) ;
#6892 = CARTESIAN_POINT ( 'NONE',  ( -60.99999999999998579, 12.46874999931720396, 1.500000000000002220 ) ) ;
#6893 = CARTESIAN_POINT ( 'NONE',  ( -61.99999999999998579, 12.40624999931720218, 2.500000000000002665 ) ) ;
#6894 = CARTESIAN_POINT ( 'NONE',  ( -62.43234176562498305, 14.72395833299193413, 0.7511620957034662593 ) ) ;
#6895 = VECTOR ( 'NONE', #2061, 1000.000000000000000 ) ;
#6896 = CARTESIAN_POINT ( 'NONE',  ( -62.86468353124999453, 9.203124999658600203, 1.500000000000002220 ) ) ;
#6897 = CARTESIAN_POINT ( 'NONE',  ( -61.99999999999998579, 15.56249999999999822, 0.5000000000000013323 ) ) ;
#6898 = CARTESIAN_POINT ( 'NONE',  ( -77.99999999999998579, -11.50000000000000711, 5.000000000000000000 ) ) ;
#6899 = CARTESIAN_POINT ( 'NONE',  ( -61.13531646874998415, 9.369791666325268054, 1.999225269531026417 ) ) ;
#6900 = VECTOR ( 'NONE', #9444, 1000.000000000000000 ) ;
#6901 = LINE ( 'NONE', #8619, #3761 ) ;
#6902 = ORIENTED_EDGE ( 'NONE', *, *, #6974, .T. ) ;
#6903 = DIRECTION ( 'NONE',  ( -0.000000000000000000, -0.000000000000000000, 1.000000000000000000 ) ) ;
#6904 = CARTESIAN_POINT ( 'NONE',  ( 0.5000000000000000000, 2.361209666477099964E-16, -1.928074011315806136 ) ) ;
#6905 = ADVANCED_FACE ( 'NONE', ( #7682 ), #6118, .F. ) ;
#6906 = AXIS2_PLACEMENT_3D ( 'NONE', #6898, #2677, #6058 ) ;
#6907 = CARTESIAN_POINT ( 'NONE',  ( -62.43234176562499016, 15.24479166632526805, 2.248837904296538071 ) ) ;
#6908 = CARTESIAN_POINT ( 'NONE',  ( -62.86468353124998032, 11.18229166632526983, 1.000774730468978246 ) ) ;
#6909 = EDGE_CURVE ( 'NONE', #4954, #8797, #9338, .T. ) ;
#6910 = CARTESIAN_POINT ( 'NONE',  ( -62.43234176562498305, 8.661458332991934128, 0.7511620957034662593 ) ) ;
#6911 =( BOUNDED_CURVE ( )  B_SPLINE_CURVE ( 2, ( #10447, #1174, #516, #6345, #1233, #3791, #3068, #9677, #8907 ),
 .UNSPECIFIED., .F., .F. ) 
 B_SPLINE_CURVE_WITH_KNOTS ( ( 3, 2, 2, 2, 3 ),
 ( 0.6953125000000000000, 0.6979166666666666297, 0.7031250000000000000, 0.7083333333333333703, 0.7109375000000000000 ),
 .UNSPECIFIED. ) 
 CURVE ( )  GEOMETRIC_REPRESENTATION_ITEM ( )  RATIONAL_B_SPLINE_CURVE ( ( 0.9330127018922194093, 0.9330127018922194093, 1.000000000000000000, 0.8660254037844387076, 1.000000000000000000, 0.8660254037844387076, 1.000000000000000000, 0.9330127018922194093, 0.9330127018922194093 ) ) 
 REPRESENTATION_ITEM ( '' )  );
#6912 = VERTEX_POINT ( 'NONE', #1899 ) ;
#6913 = CARTESIAN_POINT ( 'NONE',  ( -60.99999999999998579, 15.02083333333333393, 0.9226497308103762673 ) ) ;
#6914 = CARTESIAN_POINT ( 'NONE',  ( -61.99999999999999289, 10.07812499965860198, 2.498450539062049724 ) ) ;
#6915 = AXIS2_PLACEMENT_3D ( 'NONE', #1473, #4848, #8256 ) ;
#6916 = CARTESIAN_POINT ( 'NONE',  ( -60.99999999999998579, 13.71874999931720218, 1.500000000000002220 ) ) ;
#6917 = DIRECTION ( 'NONE',  ( 0.000000000000000000, 0.000000000000000000, -1.000000000000000000 ) ) ;
#6918 = ORIENTED_EDGE ( 'NONE', *, *, #9343, .F. ) ;
#6919 = CARTESIAN_POINT ( 'NONE',  ( -61.99999999999998579, 9.687500000000000000, 2.500000000000002665 ) ) ;
#6920 = CARTESIAN_POINT ( 'NONE',  ( -61.56765823437498852, 11.28645833299193590, 2.248837904296538515 ) ) ;
#6921 = DIRECTION ( 'NONE',  ( 0.000000000000000000, 0.000000000000000000, -1.000000000000000000 ) ) ;
#6922 = VECTOR ( 'NONE', #5147, 1000.000000000000000 ) ;
#6923 = CARTESIAN_POINT ( 'NONE',  ( 140.0000000000000284, 2.500000000000000444, 6.000000000000000000 ) ) ;
#6924 = VERTEX_POINT ( 'NONE', #5160 ) ;
#6925 = FACE_OUTER_BOUND ( 'NONE', #3809, .T. ) ;
#6926 = CARTESIAN_POINT ( 'NONE',  ( -61.99999999999998579, 12.95312499965860198, 0.5015494609379544944 ) ) ;
#6927 =( NAMED_UNIT ( * ) PLANE_ANGLE_UNIT ( ) SI_UNIT ( $, .RADIAN. ) );
#6928 = CYLINDRICAL_SURFACE ( 'NONE', #6725, 0.9999999999999981126 ) ;
#6929 = ADVANCED_FACE ( 'NONE', ( #2512, #10217 ), #116, .T. ) ;
#6930 = CARTESIAN_POINT ( 'NONE',  ( -60.99999999999998579, 9.697916665983870033, 2.077350269189628840 ) ) ;
#6931 = ORIENTED_EDGE ( 'NONE', *, *, #7200, .T. ) ;
#6932 = DIRECTION ( 'NONE',  ( -1.000000000000000000, 0.000000000000000000, 0.000000000000000000 ) ) ;
#6933 = DIRECTION ( 'NONE',  ( 0.000000000000000000, 0.000000000000000000, 1.000000000000000000 ) ) ;
#6934 = CARTESIAN_POINT ( 'NONE',  ( -61.13531646874998415, 11.59895833299193590, 1.000774730468978468 ) ) ;
#6935 = ORIENTED_EDGE ( 'NONE', *, *, #5946, .F. ) ;
#6936 = CARTESIAN_POINT ( 'NONE',  ( -62.86468353124998032, 8.744791666325268054, 1.000774730468978246 ) ) ;
#6937 = DIRECTION ( 'NONE',  ( -1.000000000000000000, -0.000000000000000000, -0.000000000000000000 ) ) ;
#6938 = CARTESIAN_POINT ( 'NONE',  ( -62.43234176562499016, 15.05729166632526805, 2.248837904296538071 ) ) ;
#6939 = CARTESIAN_POINT ( 'NONE',  ( -61.99999999999998579, 12.78124999931720218, 0.5000000000000013323 ) ) ;
#6940 = ORIENTED_EDGE ( 'NONE', *, *, #9663, .F. ) ;
#6941 = DIRECTION ( 'NONE',  ( -0.000000000000000000, -1.000000000000000000, -0.000000000000000000 ) ) ;
#6942 = EDGE_CURVE ( 'NONE', #3475, #8323, #4597, .T. ) ;
#6943 = ORIENTED_EDGE ( 'NONE', *, *, #7885, .T. ) ;
#6944 = CARTESIAN_POINT ( 'NONE',  ( -62.26794919243111082, 10.92633545031537068, 2.500000000000003109 ) ) ;
#6945 = CARTESIAN_POINT ( 'NONE',  ( -61.49999999999998579, 8.541666666666666075, 0.6339745962155628467 ) ) ;
#6946 = CARTESIAN_POINT ( 'NONE',  ( -61.99999999999998579, 8.906249999317203958, 2.500000000000002665 ) ) ;
#6947 = CARTESIAN_POINT ( 'NONE',  ( -60.99999999999998579, 10.77083333333333393, 0.9226497308103762673 ) ) ;
#6948 = CARTESIAN_POINT ( 'NONE',  ( -62.86468353124999453, 14.01562499965860198, 1.500000000000002220 ) ) ;
#6949 = CARTESIAN_POINT ( 'NONE',  ( -62.86468353124998742, 8.723958332991934128, 1.999225269531025972 ) ) ;
#6950 = CARTESIAN_POINT ( 'NONE',  ( -109.9999999999999289, 33.00000000000000711, -2.000000000000000000 ) ) ;
#6951 = FACE_OUTER_BOUND ( 'NONE', #8983, .T. ) ;
#6952 = CARTESIAN_POINT ( 'NONE',  ( -61.99999999999998579, 9.828124999658600203, 2.498450539062049724 ) ) ;
#6953 = CARTESIAN_POINT ( 'NONE',  ( -60.99999999999998579, 15.71874999931720218, 1.500000000000002220 ) ) ;
#6954 = ORIENTED_EDGE ( 'NONE', *, *, #7550, .T. ) ;
#6955 = DIRECTION ( 'NONE',  ( -0.000000000000000000, -0.000000000000000000, 1.000000000000000000 ) ) ;
#6956 = CARTESIAN_POINT ( 'NONE',  ( 145.0000000000000284, -5.500000000000000000, 3.000000000000000000 ) ) ;
#6957 = AXIS2_PLACEMENT_3D ( 'NONE', #9602, #7942, #1995 ) ;
#6958 = CARTESIAN_POINT ( 'NONE',  ( 0.5000000000000000000, 0.2499999999999998335, -1.911797424705720116 ) ) ;
#6959 = CARTESIAN_POINT ( 'NONE',  ( -61.56765823437498852, 11.53645833299193590, 2.248837904296538515 ) ) ;
#6960 = VECTOR ( 'NONE', #1558, 1000.000000000000000 ) ;
#6961 = CARTESIAN_POINT ( 'NONE',  ( -62.86468353124998032, 8.432291666325268054, 1.000774730468978024 ) ) ;
#6962 = CARTESIAN_POINT ( 'NONE',  ( -105.0000000000000000, 2.500000000000000000, 4.000000000000000000 ) ) ;
#6963 = EDGE_LOOP ( 'NONE', ( #4145, #9257 ) ) ;
#6964 = CARTESIAN_POINT ( 'NONE',  ( -60.99999999999998579, 15.50000000000000000, 1.500000000000002220 ) ) ;
#6965 = CARTESIAN_POINT ( 'NONE',  ( -62.86468353124999453, 9.515624999658600203, 1.500000000000002220 ) ) ;
#6966 =( LENGTH_UNIT ( ) NAMED_UNIT ( * ) SI_UNIT ( .MILLI., .METRE. ) );
#6967 = CARTESIAN_POINT ( 'NONE',  ( -62.86468353124999453, 14.95312499965860020, 1.500000000000002220 ) ) ;
#6968 = CARTESIAN_POINT ( 'NONE',  ( -62.49999999999998579, 12.88541666598386826, 2.366025403784441483 ) ) ;
#6969 = CARTESIAN_POINT ( 'NONE',  ( -62.26794919243111082, 14.67633545031536890, 2.500000000000003109 ) ) ;
#6970 = VERTEX_POINT ( 'NONE', #8567 ) ;
#6971 = AXIS2_PLACEMENT_3D ( 'NONE', #3670, #10169, #2566 ) ;
#6972 = AXIS2_PLACEMENT_3D ( 'NONE', #4560, #10455, #7969 ) ;
#6973 = DIRECTION ( 'NONE',  ( 1.000000000000000000, 0.000000000000000000, 0.000000000000000000 ) ) ;
#6974 = EDGE_CURVE ( 'NONE', #4962, #8694, #6846, .T. ) ;
#6975 = CARTESIAN_POINT ( 'NONE',  ( -62.86468353124999453, 11.22395833299193590, 1.999225269531025750 ) ) ;
#6976 = CYLINDRICAL_SURFACE ( 'NONE', #4039, 0.9999999999999981126 ) ;
#6977 = CARTESIAN_POINT ( 'NONE',  ( -61.73205080756886076, 15.55133545031536713, 0.5000000000000014433 ) ) ;
#6978 = ORIENTED_EDGE ( 'NONE', *, *, #9340, .F. ) ;
#6979 = CARTESIAN_POINT ( 'NONE',  ( -60.99999999999998579, 11.02083333333333570, 0.9226497308103762673 ) ) ;
#6980 = AXIS2_PLACEMENT_3D ( 'NONE', #10838, #4009, #5045 ) ;
#6981 = PLANE ( 'NONE',  #3583 ) ;
#6982 = CARTESIAN_POINT ( 'NONE',  ( -61.13531646874998415, 14.11979166632526805, 1.999225269531026417 ) ) ;
#6983 = LINE ( 'NONE', #7036, #5829 ) ;
#6984 = CARTESIAN_POINT ( 'NONE',  ( -60.99999999999998579, 9.239583332650534331, 0.9226497308103762673 ) ) ;
#6985 = ORIENTED_EDGE ( 'NONE', *, *, #9765, .T. ) ;
#6986 = CARTESIAN_POINT ( 'NONE',  ( -60.99999999999998579, 13.52083333333333215, 0.9226497308103762673 ) ) ;
#6987 = VECTOR ( 'NONE', #6164, 1000.000000000000000 ) ;
#6988 = DIRECTION ( 'NONE',  ( 0.000000000000000000, 0.000000000000000000, 1.000000000000000000 ) ) ;
#6989 = CARTESIAN_POINT ( 'NONE',  ( -61.56765823437498852, 11.78645833299193413, 2.248837904296538515 ) ) ;
#6990 = EDGE_CURVE ( 'NONE', #2594, #3363, #2565, .T. ) ;
#6991 = ORIENTED_EDGE ( 'NONE', *, *, #141, .T. ) ;
#6992 = CARTESIAN_POINT ( 'NONE',  ( -62.86468353124998032, 9.994791666325268054, 1.000774730468978246 ) ) ;
#6993 = CARTESIAN_POINT ( 'NONE',  ( -61.99999999999998579, 16.00000000000000000, 1.500000000000002220 ) ) ;
#6994 = CIRCLE ( 'NONE', #1025, 1.000000000000000888 ) ;
#6995 = CARTESIAN_POINT ( 'NONE',  ( -61.13531646874998415, 14.86979166632526805, 1.999225269531026417 ) ) ;
#6996 = CARTESIAN_POINT ( 'NONE',  ( -79.09999999999998010, 11.49999999999999645, -2.000000000000001332 ) ) ;
#6997 = ORIENTED_EDGE ( 'NONE', *, *, #2100, .T. ) ;
#6998 = DIRECTION ( 'NONE',  ( 0.000000000000000000, 0.000000000000000000, -1.000000000000000000 ) ) ;
#6999 = B_SPLINE_CURVE_WITH_KNOTS ( 'NONE', 3,
 ( #3103, #9939, #2483, #8318, #8480, #813 ),
 .UNSPECIFIED., .F., .F.,
 ( 4, 2, 4 ),
 ( 0.002363858439908544419, 0.002786031303543298580, 0.003208204167178053175 ),
 .UNSPECIFIED. ) ;
#7000 = ORIENTED_EDGE ( 'NONE', *, *, #1485, .T. ) ;
#7001 = DIRECTION ( 'NONE',  ( 0.000000000000000000, -0.000000000000000000, -1.000000000000000000 ) ) ;
#7002 = CARTESIAN_POINT ( 'NONE',  ( -62.49999999999998579, 8.083333333333332149, 0.6339745962155627357 ) ) ;
#7003 = DIRECTION ( 'NONE',  ( 0.000000000000000000, 0.000000000000000000, -1.000000000000000000 ) ) ;
#7004 = CARTESIAN_POINT ( 'NONE',  ( -61.99999999999998579, 10.68749999999999822, 2.500000000000002665 ) ) ;
#7005 = CARTESIAN_POINT ( 'NONE',  ( -61.99999999999998579, 16.00000000000000000, 1.500000000000002220 ) ) ;
#7006 = CARTESIAN_POINT ( 'NONE',  ( -61.99999999999999289, 13.70312499965860198, 0.5015494609379544944 ) ) ;
#7007 = CARTESIAN_POINT ( 'NONE',  ( -62.86468353124998032, 9.182291666325268054, 1.000774730468978246 ) ) ;
#7008 = CARTESIAN_POINT ( 'NONE',  ( -61.99999999999998579, 10.81250000000000000, 0.5000000000000013323 ) ) ;
#7009 = CARTESIAN_POINT ( 'NONE',  ( -120.0000000000000000, -4.000000000000019540, -2.000000000000000000 ) ) ;
#7010 = CARTESIAN_POINT ( 'NONE',  ( -61.13531646874998415, 10.41145833299193413, 1.000774730468978468 ) ) ;
#7011 = FACE_OUTER_BOUND ( 'NONE', #7592, .T. ) ;
#7012 = ORIENTED_EDGE ( 'NONE', *, *, #7089, .T. ) ;
#7013 = CARTESIAN_POINT ( 'NONE',  ( -61.49999999999998579, 14.01041666598387003, 0.6339745962155628467 ) ) ;
#7014 = CARTESIAN_POINT ( 'NONE',  ( -62.49999999999998579, 11.33333333333333393, 0.6339745962155627357 ) ) ;
#7015 = CARTESIAN_POINT ( 'NONE',  ( -62.43234176562498305, 12.16145833299193413, 0.7511620957034662593 ) ) ;
#7016 = CARTESIAN_POINT ( 'NONE',  ( -61.99999999999999289, 9.265624999658598426, 2.498450539062049724 ) ) ;
#7017 = CARTESIAN_POINT ( 'NONE',  ( -61.99999999999997868, 9.781249999317202182, 0.5000000000000013323 ) ) ;
#7018 = EDGE_LOOP ( 'NONE', ( #9185, #10582, #7485, #3026 ) ) ;
#7019 = CARTESIAN_POINT ( 'NONE',  ( -62.49999999999998579, 15.91666666666666607, 2.366025403784441483 ) ) ;
#7020 = CARTESIAN_POINT ( 'NONE',  ( -61.99999999999999289, 10.57812499965860198, 2.498450539062049724 ) ) ;
#7021 = DIRECTION ( 'NONE',  ( 0.000000000000000000, 0.000000000000000000, 1.000000000000000000 ) ) ;
#7022 = CARTESIAN_POINT ( 'NONE',  ( -62.86468353124998032, 14.93229166632526983, 1.000774730468978246 ) ) ;
#7023 = ADVANCED_FACE ( 'NONE', ( #5901 ), #1683, .F. ) ;
#7024 = EDGE_CURVE ( 'NONE', #3356, #24, #5847, .T. ) ;
#7025 = CARTESIAN_POINT ( 'NONE',  ( -60.99999999999998579, 14.71874999931720218, 1.500000000000002220 ) ) ;
#7026 = DIRECTION ( 'NONE',  ( 0.000000000000000000, 0.000000000000000000, -1.000000000000000000 ) ) ;
#7027 = ORIENTED_EDGE ( 'NONE', *, *, #5925, .F. ) ;
#7028 = CARTESIAN_POINT ( 'NONE',  ( -62.49999999999998579, 11.58333333333333393, 0.6339745962155627357 ) ) ;
#7029 = CARTESIAN_POINT ( 'NONE',  ( -62.43234176562498305, 10.91145833299193413, 0.7511620957034662593 ) ) ;
#7030 = CARTESIAN_POINT ( 'NONE',  ( -62.43234176562499016, 8.744791666325268054, 2.248837904296538071 ) ) ;
#7031 = CARTESIAN_POINT ( 'NONE',  ( 1.299999999999999156, 0.000000000000000000, 1.000000000000000000 ) ) ;
#7032 = ORIENTED_EDGE ( 'NONE', *, *, #9600, .T. ) ;
#7033 = CARTESIAN_POINT ( 'NONE',  ( -62.99999999999998579, 11.35416666666666785, 0.9226497308103756012 ) ) ;
#7034 = LINE ( 'NONE', #7986, #10318 ) ;
#7035 = CARTESIAN_POINT ( 'NONE',  ( -62.43234176562499016, 13.80729166632526805, 2.248837904296538071 ) ) ;
#7036 = CARTESIAN_POINT ( 'NONE',  ( -120.0000000000000000, 14.99999999999998579, 83.15773105863907233 ) ) ;
#7037 = CARTESIAN_POINT ( 'NONE',  ( -61.99999999999998579, 11.15624999931720396, 2.654700538379254571 ) ) ;
#7038 = ORIENTED_EDGE ( 'NONE', *, *, #3130, .F. ) ;
#7039 = CARTESIAN_POINT ( 'NONE',  ( -61.99999999999998579, 13.93749999999999822, 2.500000000000002665 ) ) ;
#7040 = DIRECTION ( 'NONE',  ( 0.000000000000000000, -0.000000000000000000, -1.000000000000000000 ) ) ;
#7041 = CARTESIAN_POINT ( 'NONE',  ( -61.13531646874998415, 11.34895833299193413, 1.000774730468978468 ) ) ;
#7042 = EDGE_CURVE ( 'NONE', #424, #2359, #1730, .T. ) ;
#7043 = VERTEX_POINT ( 'NONE', #5106 ) ;
#7044 = ADVANCED_FACE ( 'NONE', ( #11 ), #5952, .F. ) ;
#7045 = CARTESIAN_POINT ( 'NONE',  ( -62.86468353124999453, 10.51562499965860198, 1.500000000000002220 ) ) ;
#7046 = CARTESIAN_POINT ( 'NONE',  ( -62.99999999999998579, 15.57291666598387003, 0.9226497308103756012 ) ) ;
#7047 = CARTESIAN_POINT ( 'NONE',  ( -61.56765823437498142, 14.43229166632526983, 0.7511620957034663704 ) ) ;
#7048 = CARTESIAN_POINT ( 'NONE',  ( -61.99999999999998579, 8.906249999317203958, 2.500000000000002665 ) ) ;
#7049 = VERTEX_POINT ( 'NONE', #462 ) ;
#7050 = CARTESIAN_POINT ( 'NONE',  ( -149.9999999999999716, 8.000000000000000000, 0.000000000000000000 ) ) ;
#7051 = COLOUR_RGB ( '',0.8941176470588234615, 0.8941176470588234615, 0.8941176470588234615 ) ;
#7052 = ORIENTED_EDGE ( 'NONE', *, *, #8209, .F. ) ;
#7053 = PLANE ( 'NONE',  #6790 ) ;
#7054 = CARTESIAN_POINT ( 'NONE',  ( -60.99999999999998579, 9.020833333333333925, 0.9226497308103762673 ) ) ;
#7055 = DIRECTION ( 'NONE',  ( 0.7071067811865472397, 0.000000000000000000, 0.7071067811865479058 ) ) ;
#7056 = CARTESIAN_POINT ( 'NONE',  ( -61.99999999999998579, 12.40624999931720218, 2.500000000000002665 ) ) ;
#7057 = CARTESIAN_POINT ( 'NONE',  ( -42.47213595499957961, -18.00000000000001066, 5.000000000000000000 ) ) ;
#7058 = CARTESIAN_POINT ( 'NONE',  ( -61.99999999999999289, 14.32812499965860020, 2.498450539062049724 ) ) ;
#7059 = CARTESIAN_POINT ( 'NONE',  ( -61.99999999999998579, 10.01562499965860020, 2.498450539062049724 ) ) ;
#7060 = DIRECTION ( 'NONE',  ( -0.000000000000000000, -1.000000000000000000, -0.000000000000000000 ) ) ;
#7061 = EDGE_CURVE ( 'NONE', #10637, #8021, #2584, .T. ) ;
#7062 = COLOUR_RGB ( '',0.8941176470588234615, 0.8941176470588234615, 0.8941176470588234615 ) ;
#7063 = CARTESIAN_POINT ( 'NONE',  ( -62.43234176562499016, 10.80729166632526805, 2.248837904296538071 ) ) ;
#7064 = CARTESIAN_POINT ( 'NONE',  ( -60.99999999999998579, 8.109374999658601979, 1.500000000000002220 ) ) ;
#7065 = VERTEX_POINT ( 'NONE', #10391 ) ;
#7066 = DIRECTION ( 'NONE',  ( 0.000000000000000000, 0.000000000000000000, -1.000000000000000000 ) ) ;
#7067 = CARTESIAN_POINT ( 'NONE',  ( -61.49999999999998579, 15.20833333333333393, 2.366025403784441927 ) ) ;
#7068 =( BOUNDED_CURVE ( )  B_SPLINE_CURVE ( 2, ( #2430, #2280, #9219, #6566, #8327, #9948, #10827, #9110, #5608 ),
 .UNSPECIFIED., .F., .T. ) 
 B_SPLINE_CURVE_WITH_KNOTS ( ( 3, 2, 2, 2, 3 ),
 ( 0.8359375000000000000, 0.8385416666666666297, 0.8437500000000000000, 0.8489583333333333703, 0.8515625000000000000 ),
 .UNSPECIFIED. ) 
 CURVE ( )  GEOMETRIC_REPRESENTATION_ITEM ( )  RATIONAL_B_SPLINE_CURVE ( ( 0.9330127018922194093, 0.9330127018922194093, 1.000000000000000000, 0.8660254037844387076, 1.000000000000000000, 0.8660254037844387076, 1.000000000000000000, 0.9330127018922194093, 0.9330127018922194093 ) ) 
 REPRESENTATION_ITEM ( '' )  );
#7069 = CARTESIAN_POINT ( 'NONE',  ( -62.99999999999998579, 10.07291666598387003, 0.9226497308103756012 ) ) ;
#7070 = CARTESIAN_POINT ( 'NONE',  ( -62.43234176562499016, 12.99479166632526805, 2.248837904296538071 ) ) ;
#7071 = VECTOR ( 'NONE', #9961, 1000.000000000000000 ) ;
#7072 = CARTESIAN_POINT ( 'NONE',  ( -62.43234176562499016, 8.244791666325268054, 2.248837904296538071 ) ) ;
#7073 = EDGE_CURVE ( 'NONE', #5247, #9306, #9575, .T. ) ;
#7074 = LINE ( 'NONE', #9629, #148 ) ;
#7075 = VERTEX_POINT ( 'NONE', #8909 ) ;
#7076 = CARTESIAN_POINT ( 'NONE',  ( -61.99999999999997868, 10.90624999931720218, 2.500000000000002665 ) ) ;
#7077 = CARTESIAN_POINT ( 'NONE',  ( -61.56765823437498142, 10.43229166632526983, 0.7511620957034663704 ) ) ;
#7078 = AXIS2_PLACEMENT_3D ( 'NONE', #1501, #512, #4100 ) ;
#7079 = SHAPE_DEFINITION_REPRESENTATION ( #9196, #560 ) ;
#7080 = CARTESIAN_POINT ( 'NONE',  ( -62.86468353124999453, 15.70312499965860198, 1.500000000000002220 ) ) ;
#7081 = CARTESIAN_POINT ( 'NONE',  ( -61.99999999999998579, 14.90624999931720218, 2.654700538379254571 ) ) ;
#7082 = FACE_OUTER_BOUND ( 'NONE', #4518, .T. ) ;
#7083 = VERTEX_POINT ( 'NONE', #10449 ) ;
#7084 = ADVANCED_FACE ( 'NONE', ( #6409 ), #6295, .T. ) ;
#7085 = LINE ( 'NONE', #3748, #1819 ) ;
#7086 = VECTOR ( 'NONE', #7708, 1000.000000000000000 ) ;
#7087 = ORIENTED_EDGE ( 'NONE', *, *, #6766, .F. ) ;
#7088 = CARTESIAN_POINT ( 'NONE',  ( -61.56765823437498142, 12.36979166632526805, 0.7511620957034663704 ) ) ;
#7089 = EDGE_CURVE ( 'NONE', #427, #4976, #5565, .T. ) ;
#7090 = CARTESIAN_POINT ( 'NONE',  ( -62.43234176562498305, 8.911458332991934128, 0.7511620957034662593 ) ) ;
#7091 = DIRECTION ( 'NONE',  ( 0.000000000000000000, 1.000000000000000000, 0.000000000000000000 ) ) ;
#7092 = ORIENTED_EDGE ( 'NONE', *, *, #5919, .F. ) ;
#7093 = CARTESIAN_POINT ( 'NONE',  ( -62.99999999999998579, 12.14583333333333393, 2.077350269189627952 ) ) ;
#7094 = DIRECTION ( 'NONE',  ( 0.000000000000000000, 0.000000000000000000, -1.000000000000000000 ) ) ;
#7095 = VECTOR ( 'NONE', #7820, 1000.000000000000000 ) ;
#7096 = CARTESIAN_POINT ( 'NONE',  ( -61.13531646874998415, 14.41145833299193413, 1.000774730468978468 ) ) ;
#7097 = CARTESIAN_POINT ( 'NONE',  ( -62.99999999999998579, 13.85416666666666785, 0.9226497308103756012 ) ) ;
#7098 = CARTESIAN_POINT ( 'NONE',  ( -62.49999999999998579, 10.30208333265053611, 0.6339745962155627357 ) ) ;
#7099 = VECTOR ( 'NONE', #5438, 1000.000000000000000 ) ;
#7100 = VERTEX_POINT ( 'NONE', #10565 ) ;
#7101 = FACE_OUTER_BOUND ( 'NONE', #1316, .T. ) ;
#7102 = LINE ( 'NONE', #2880, #3497 ) ;
#7103 = VECTOR ( 'NONE', #7721, 1000.000000000000000 ) ;
#7104 = CARTESIAN_POINT ( 'NONE',  ( -62.43234176562499016, 12.24479166632526805, 2.248837904296538071 ) ) ;
#7105 = SURFACE_SIDE_STYLE ('',( #5477 ) ) ;
#7106 = ORIENTED_EDGE ( 'NONE', *, *, #792, .T. ) ;
#7107 = CARTESIAN_POINT ( 'NONE',  ( -61.13531646874998415, 10.61979166632526983, 1.999225269531026417 ) ) ;
#7108 = PLANE ( 'NONE',  #6716 ) ;
#7109 = VECTOR ( 'NONE', #5602, 1000.000000000000000 ) ;
#7110 = CARTESIAN_POINT ( 'NONE',  ( -61.13531646874998415, 14.11979166632526805, 1.999225269531026417 ) ) ;
#7111 = PLANE ( 'NONE',  #6264 ) ;
#7112 = ORIENTED_EDGE ( 'NONE', *, *, #6549, .T. ) ;
#7113 = PLANE ( 'NONE',  #5856 ) ;
#7114 = EDGE_CURVE ( 'NONE', #6102, #3881, #5673, .T. ) ;
#7115 = ORIENTED_EDGE ( 'NONE', *, *, #9918, .T. ) ;
#7116 = FACE_OUTER_BOUND ( 'NONE', #814, .T. ) ;
#7117 = CARTESIAN_POINT ( 'NONE',  ( -62.99999999999998579, 8.854166666666667851, 0.9226497308103756012 ) ) ;
#7118 = LINE ( 'NONE', #8009, #64 ) ;
#7119 = CARTESIAN_POINT ( 'NONE',  ( -60.99999999999998579, 16.19791666598386826, 2.077350269189628840 ) ) ;
#7120 = DIRECTION ( 'NONE',  ( 0.000000000000000000, 0.000000000000000000, 1.000000000000000000 ) ) ;
#7121 = CARTESIAN_POINT ( 'NONE',  ( -62.43234176562498305, 14.22395833299193413, 0.7511620957034662593 ) ) ;
#7122 = CARTESIAN_POINT ( 'NONE',  ( -61.13531646874998415, 10.34895833299193413, 1.000774730468978468 ) ) ;
#7123 = LINE ( 'NONE', #6290, #9745 ) ;
#7124 = DIRECTION ( 'NONE',  ( 0.000000000000000000, -6.217248937900875838E-15, 1.000000000000000000 ) ) ;
#7125 = CARTESIAN_POINT ( 'NONE',  ( -62.86468353124998742, 10.53645833299193413, 1.999225269531025972 ) ) ;
#7126 = DIRECTION ( 'NONE',  ( 1.000000000000000000, 0.000000000000000000, -0.000000000000000000 ) ) ;
#7127 = ORIENTED_EDGE ( 'NONE', *, *, #5472, .T. ) ;
#7128 = CARTESIAN_POINT ( 'NONE',  ( -62.99999999999998579, 14.35416666666666785, 0.9226497308103756012 ) ) ;
#7129 = DIRECTION ( 'NONE',  ( 1.000000000000000000, 0.000000000000000000, 0.000000000000000000 ) ) ;
#7130 = ORIENTED_EDGE ( 'NONE', *, *, #9373, .F. ) ;
#7131 = CARTESIAN_POINT ( 'NONE',  ( -61.99999999999998579, 16.00000000000000000, 2.500000000000000444 ) ) ;
#7132 = EDGE_CURVE ( 'NONE', #9455, #1136, #2963, .T. ) ;
#7133 = CARTESIAN_POINT ( 'NONE',  ( -61.13531646874998415, 12.09895833299193235, 1.000774730468978468 ) ) ;
#7134 = CARTESIAN_POINT ( 'NONE',  ( -61.13531646874997705, 10.55729166632526805, 1.999225269531026417 ) ) ;
#7135 = FILL_AREA_STYLE ('',( #352 ) ) ;
#7136 = EDGE_LOOP ( 'NONE', ( #1570, #3298 ) ) ;
#7137 = CARTESIAN_POINT ( 'NONE',  ( -60.99999999999998579, 8.489583332650536107, 0.9226497308103762673 ) ) ;
#7138 = AXIS2_PLACEMENT_3D ( 'NONE', #6138, #1863, #1805 ) ;
#7139 = CARTESIAN_POINT ( 'NONE',  ( -62.43234176562499016, 10.55729166632526983, 2.248837904296538071 ) ) ;
#7140 = APPLICATION_PROTOCOL_DEFINITION ( 'draft international standard', 'automotive_design', 1998, #10293 ) ;
#7141 = CARTESIAN_POINT ( 'NONE',  ( -61.13531646874998415, 15.32812499965860020, 1.500000000000002220 ) ) ;
#7142 = CARTESIAN_POINT ( 'NONE',  ( -62.49999999999998579, 15.13541666598387003, 2.366025403784441483 ) ) ;
#7143 = CARTESIAN_POINT ( 'NONE',  ( -61.49999999999998579, 14.76041666598386826, 0.6339745962155628467 ) ) ;
#7144 = ORIENTED_EDGE ( 'NONE', *, *, #4382, .T. ) ;
#7145 = ORIENTED_EDGE ( 'NONE', *, *, #118, .F. ) ;
#7146 =( BOUNDED_CURVE ( )  B_SPLINE_CURVE ( 2, ( #3815, #7205, #4693, #3869, #3923, #2983, #3091, #6369, #543 ),
 .UNSPECIFIED., .F., .T. ) 
 B_SPLINE_CURVE_WITH_KNOTS ( ( 3, 2, 2, 2, 3 ),
 ( 0.4609375000000000000, 0.4635416666666666852, 0.4687500000000000000, 0.4739583333333333148, 0.4765625000000000000 ),
 .UNSPECIFIED. ) 
 CURVE ( )  GEOMETRIC_REPRESENTATION_ITEM ( )  RATIONAL_B_SPLINE_CURVE ( ( 0.9330127018922194093, 0.9330127018922194093, 1.000000000000000000, 0.8660254037844387076, 1.000000000000000000, 0.8660254037844387076, 1.000000000000000000, 0.9330127018922194093, 0.9330127018922194093 ) ) 
 REPRESENTATION_ITEM ( '' )  );
#7147 = VECTOR ( 'NONE', #7469, 1000.000000000000000 ) ;
#7148 = CARTESIAN_POINT ( 'NONE',  ( -61.13531646874998415, 12.82812499965860198, 1.500000000000002220 ) ) ;
#7149 = CARTESIAN_POINT ( 'NONE',  ( -62.86468353124999453, 8.203124999658601979, 1.500000000000002220 ) ) ;
#7150 = CARTESIAN_POINT ( 'NONE',  ( -62.49999999999998579, 10.63541666598387003, 2.366025403784441483 ) ) ;
#7151 = ORIENTED_EDGE ( 'NONE', *, *, #5807, .F. ) ;
#7152 = CARTESIAN_POINT ( 'NONE',  ( -61.99999999999998579, 12.56250000000000178, 0.3452994616207497591 ) ) ;
#7153 = CARTESIAN_POINT ( 'NONE',  ( -61.99999999999998579, 14.70312499965860020, 0.5015494609379544944 ) ) ;
#7154 = AXIS2_PLACEMENT_3D ( 'NONE', #6514, #1400, #1552 ) ;
#7155 = CARTESIAN_POINT ( 'NONE',  ( -62.99999999999998579, 10.34374999931720218, 1.500000000000001998 ) ) ;
#7156 = VERTEX_POINT ( 'NONE', #6347 ) ;
#7157 = DIRECTION ( 'NONE',  ( 1.000000000000000000, 0.000000000000000000, 0.000000000000000000 ) ) ;
#7158 = CARTESIAN_POINT ( 'NONE',  ( -61.99999999999998579, 10.40624999931720218, 2.500000000000002665 ) ) ;
#7159 = CARTESIAN_POINT ( 'NONE',  ( -61.13531646874998415, 12.09895833299193235, 1.000774730468978468 ) ) ;
#7160 = CARTESIAN_POINT ( 'NONE',  ( 140.0000000000000284, 8.000000000000000000, 6.000000000000000000 ) ) ;
#7161 = EDGE_LOOP ( 'NONE', ( #8724, #4746, #8965, #5670 ) ) ;
#7162 = CARTESIAN_POINT ( 'NONE',  ( -61.56765823437498852, 10.84895833299193413, 2.248837904296538515 ) ) ;
#7163 = CARTESIAN_POINT ( 'NONE',  ( -139.9999999999999716, -8.000000000000000000, 3.000000000000000000 ) ) ;
#7164 = AXIS2_PLACEMENT_3D ( 'NONE', #10566, #5566, #10680 ) ;
#7165 = EDGE_CURVE ( 'NONE', #6452, #6102, #2314, .T. ) ;
#7166 = CARTESIAN_POINT ( 'NONE',  ( -62.43234176562499016, 14.80729166632526805, 2.248837904296538071 ) ) ;
#7167 = LINE ( 'NONE', #10550, #9986 ) ;
#7168 = ORIENTED_EDGE ( 'NONE', *, *, #821, .F. ) ;
#7169 = CARTESIAN_POINT ( 'NONE',  ( -62.99999999999998579, 9.375000000000000000, 1.500000000000001998 ) ) ;
#7170 = ORIENTED_EDGE ( 'NONE', *, *, #6064, .F. ) ;
#7171 = DIRECTION ( 'NONE',  ( 1.000000000000000000, 0.000000000000000000, 0.000000000000000000 ) ) ;
#7172 = CARTESIAN_POINT ( 'NONE',  ( -62.49999999999998579, 8.916666666666666075, 2.366025403784441483 ) ) ;
#7173 = LINE ( 'NONE', #10668, #5374 ) ;
#7174 = LINE ( 'NONE', #1110, #10613 ) ;
#7175 = LINE ( 'NONE', #7057, #7768 ) ;
#7176 = CARTESIAN_POINT ( 'NONE',  ( -62.86468353124998032, 9.682291666325266277, 1.000774730468978246 ) ) ;
#7177 = ADVANCED_FACE ( 'NONE', ( #285, #8849, #3669 ), #9679, .F. ) ;
#7178 = DIRECTION ( 'NONE',  ( -0.000000000000000000, -0.000000000000000000, -1.000000000000000000 ) ) ;
#7179 = CARTESIAN_POINT ( 'NONE',  ( -61.99999999999998579, 16.00000000000000000, 2.500000000000000444 ) ) ;
#7180 = CARTESIAN_POINT ( 'NONE',  ( -61.99999999999998579, 10.20312499965860198, 0.5015494609379544944 ) ) ;
#7181 = CARTESIAN_POINT ( 'NONE',  ( 150.0000000000000284, 2.500000000000000000, 2.000000000000000000 ) ) ;
#7182 = ORIENTED_EDGE ( 'NONE', *, *, #826, .T. ) ;
#7183 = CARTESIAN_POINT ( 'NONE',  ( -61.99999999999998579, 14.03124999931720218, 0.5000000000000013323 ) ) ;
#7184 = DIRECTION ( 'NONE',  ( -1.000000000000000000, -0.000000000000000000, -0.000000000000000000 ) ) ;
#7185 = ORIENTED_EDGE ( 'NONE', *, *, #3260, .F. ) ;
#7186 = CARTESIAN_POINT ( 'NONE',  ( -60.99999999999998579, 15.75000000000000000, 1.500000000000002220 ) ) ;
#7187 = EDGE_CURVE ( 'NONE', #8978, #8454, #8440, .T. ) ;
#7188 = CARTESIAN_POINT ( 'NONE',  ( -61.56765823437498852, 12.03645833299193413, 2.248837904296538515 ) ) ;
#7189 = CARTESIAN_POINT ( 'NONE',  ( -62.43234176562498305, 10.16145833299193413, 0.7511620957034662593 ) ) ;
#7190 = DIRECTION ( 'NONE',  ( -0.000000000000000000, -1.000000000000000000, -0.000000000000000000 ) ) ;
#7191 = ORIENTED_EDGE ( 'NONE', *, *, #4985, .F. ) ;
#7192 = CARTESIAN_POINT ( 'NONE',  ( -61.49999999999998579, 15.95833333333333215, 2.366025403784441927 ) ) ;
#7193 = CARTESIAN_POINT ( 'NONE',  ( -61.99999999999999289, 10.82812499965860198, 2.498450539062049724 ) ) ;
#7194 = EDGE_CURVE ( 'NONE', #1253, #1578, #10275, .T. ) ;
#7195 = APPLICATION_PROTOCOL_DEFINITION ( 'draft international standard', 'automotive_design', 1998, #3715 ) ;
#7196 = CARTESIAN_POINT ( 'NONE',  ( -61.13531646874998415, 15.07812499965860020, 1.500000000000002220 ) ) ;
#7197 = CARTESIAN_POINT ( 'NONE',  ( -62.99999999999998579, 14.07291666598387003, 0.9226497308103756012 ) ) ;
#7198 = LINE ( 'NONE', #477, #1656 ) ;
#7199 = ORIENTED_EDGE ( 'NONE', *, *, #6412, .F. ) ;
#7200 = EDGE_CURVE ( 'NONE', #8261, #8575, #5507, .T. ) ;
#7201 = CARTESIAN_POINT ( 'NONE',  ( -61.73205080756886076, 15.16741454900183328, 2.500000000000003109 ) ) ;
#7202 = ORIENTED_EDGE ( 'NONE', *, *, #7761, .T. ) ;
#7203 = CARTESIAN_POINT ( 'NONE',  ( -61.13531646874998415, 13.32812499965860020, 1.500000000000002220 ) ) ;
#7204 = CARTESIAN_POINT ( 'NONE',  ( -61.13531646874998415, 8.078124999658601979, 1.500000000000002220 ) ) ;
#7205 = CARTESIAN_POINT ( 'NONE',  ( -61.73205080756886076, 11.69866454968463110, 2.500000000000003109 ) ) ;
#7206 = ORIENTED_EDGE ( 'NONE', *, *, #9373, .T. ) ;
#7207 = CARTESIAN_POINT ( 'NONE',  ( -62.99999999999998579, 12.12500000000000000, 1.500000000000001998 ) ) ;
#7208 = CARTESIAN_POINT ( 'NONE',  ( -60.99999999999998579, 14.97916666666666430, 2.077350269189628840 ) ) ;
#7209 = CARTESIAN_POINT ( 'NONE',  ( -61.49999999999998579, 11.17708333265053611, 2.366025403784441927 ) ) ;
#7210 = EDGE_LOOP ( 'NONE', ( #10957, #5020, #2350, #1078 ) ) ;
#7211 =( BOUNDED_CURVE ( )  B_SPLINE_CURVE ( 2, ( #163, #10322, #8727, #4434, #8610, #4316, #2671, #7726, #6946 ),
 .UNSPECIFIED., .F., .T. ) 
 B_SPLINE_CURVE_WITH_KNOTS ( ( 3, 2, 2, 2, 3 ),
 ( 0.07031250000000001388, 0.07291666666666667129, 0.07812500000000000000, 0.08333333333333332871, 0.08593750000000000000 ),
 .UNSPECIFIED. ) 
 CURVE ( )  GEOMETRIC_REPRESENTATION_ITEM ( )  RATIONAL_B_SPLINE_CURVE ( ( 0.9330127018922192983, 0.9330127018922196314, 1.000000000000000000, 0.8660254037844387076, 1.000000000000000000, 0.8660254037844387076, 1.000000000000000000, 0.9330127018922194093, 0.9330127018922194093 ) ) 
 REPRESENTATION_ITEM ( '' )  );
#7212 = CARTESIAN_POINT ( 'NONE',  ( 0.05007909176323183803, -0.2500000000000001665, 1.595164775286566305 ) ) ;
#7213 = CARTESIAN_POINT ( 'NONE',  ( -61.13531646874998415, 13.07812499965860198, 1.500000000000002220 ) ) ;
#7214 = CARTESIAN_POINT ( 'NONE',  ( -61.99999999999998579, 15.93749999999999645, 2.500000000000002665 ) ) ;
#7215 = EDGE_LOOP ( 'NONE', ( #4622, #8272, #715 ) ) ;
#7216 = CARTESIAN_POINT ( 'NONE',  ( -62.43234176562499016, 10.80729166632526805, 2.248837904296538071 ) ) ;
#7217 = EDGE_CURVE ( 'NONE', #1148, #4783, #5494, .T. ) ;
#7218 = CARTESIAN_POINT ( 'NONE',  ( -62.99999999999998579, 12.59374999931720396, 1.500000000000001998 ) ) ;
#7219 = CARTESIAN_POINT ( 'NONE',  ( -61.13531646874998415, 15.91145833299193590, 1.000774730468978468 ) ) ;
#7220 = LINE ( 'NONE', #1216, #7673 ) ;
#7221 = ORIENTED_EDGE ( 'NONE', *, *, #8394, .T. ) ;
#7222 = EDGE_CURVE ( 'NONE', #5865, #4030, #5671, .T. ) ;
#7223 = DIRECTION ( 'NONE',  ( 0.000000000000000000, 0.000000000000000000, -1.000000000000000000 ) ) ;
#7224 = ORIENTED_EDGE ( 'NONE', *, *, #1371, .F. ) ;
#7225 = CARTESIAN_POINT ( 'NONE',  ( -149.9999999999999716, 8.000000000000000000, 3.000000000000000000 ) ) ;
#7226 = EDGE_CURVE ( 'NONE', #5688, #3585, #518, .T. ) ;
#7227 = CARTESIAN_POINT ( 'NONE',  ( -61.49999999999998579, 10.29166666666666785, 0.6339745962155628467 ) ) ;
#7228 = PLANE ( 'NONE',  #5567 ) ;
#7229 = DIRECTION ( 'NONE',  ( -0.8660254037844418162, 0.4999999999999947264, -0.000000000000000000 ) ) ;
#7230 = CARTESIAN_POINT ( 'NONE',  ( -79.09999999999999432, -11.50000000000000711, 4.999999999999999112 ) ) ;
#7231 = CARTESIAN_POINT ( 'NONE',  ( -62.86468353124999453, 10.45312499965860198, 1.500000000000002220 ) ) ;
#7232 = DIRECTION ( 'NONE',  ( 0.000000000000000000, 0.000000000000000000, -1.000000000000000000 ) ) ;
#7233 = CARTESIAN_POINT ( 'NONE',  ( -61.56765823437498142, 11.18229166632526805, 0.7511620957034663704 ) ) ;
#7234 = CARTESIAN_POINT ( 'NONE',  ( -62.99999999999998579, 12.14583333333333393, 2.077350269189627952 ) ) ;
#7235 = VERTEX_POINT ( 'NONE', #3217 ) ;
#7236 = CARTESIAN_POINT ( 'NONE',  ( -60.99999999999998579, 13.96874999931720218, 1.500000000000002220 ) ) ;
#7237 = CARTESIAN_POINT ( 'NONE',  ( -99.99999999999998579, 15.67949192431120053, -2.000000000000000000 ) ) ;
#7238 = AXIS2_PLACEMENT_3D ( 'NONE', #2215, #2263, #5593 ) ;
#7239 = EDGE_LOOP ( 'NONE', ( #6640, #9170, #7553, #7151 ) ) ;
#7240 = CARTESIAN_POINT ( 'NONE',  ( -60.99999999999998579, 9.979166666666667851, 2.077350269189628840 ) ) ;
#7241 = CARTESIAN_POINT ( 'NONE',  ( -62.86468353124998742, 14.47395833299193413, 1.999225269531025972 ) ) ;
#7242 = CARTESIAN_POINT ( 'NONE',  ( -61.13531646874997705, 9.598958332991934128, 1.000774730468978468 ) ) ;
#7243 = SURFACE_SIDE_STYLE ('',( #2242 ) ) ;
#7244 = ORIENTED_EDGE ( 'NONE', *, *, #3607, .T. ) ;
#7245 = CARTESIAN_POINT ( 'NONE',  ( -62.99999999999998579, 15.87500000000000000, 1.500000000000001998 ) ) ;
#7246 = CARTESIAN_POINT ( 'NONE',  ( -61.13531646874998415, 11.64062499965860198, 1.500000000000002220 ) ) ;
#7247 = SHAPE_DEFINITION_REPRESENTATION ( #1556, #10405 ) ;
#7248 = CARTESIAN_POINT ( 'NONE',  ( -105.0000000000000000, 2.500000000000000000, 4.000000000000000000 ) ) ;
#7249 = CARTESIAN_POINT ( 'NONE',  ( -62.99999999999998579, 14.59374999931720218, 1.500000000000001998 ) ) ;
#7250 = CARTESIAN_POINT ( 'NONE',  ( -61.99999999999998579, 8.000000000000000000, 2.500000000000000444 ) ) ;
#7251 = VERTEX_POINT ( 'NONE', #1454 ) ;
#7252 = EDGE_CURVE ( 'NONE', #9653, #9204, #2435, .T. ) ;
#7253 = CARTESIAN_POINT ( 'NONE',  ( -149.9999999999999716, -12.99999999999998757, 3.000000000000000000 ) ) ;
#7254 = ORIENTED_EDGE ( 'NONE', *, *, #1855, .F. ) ;
#7255 = COLOUR_RGB ( '',0.8941176470588234615, 0.8941176470588234615, 0.8941176470588234615 ) ;
#7256 = EDGE_CURVE ( 'NONE', #7667, #3055, #2111, .T. ) ;
#7257 = CARTESIAN_POINT ( 'NONE',  ( -62.86468353124999453, 13.45312499965860020, 1.500000000000002220 ) ) ;
#7258 = CARTESIAN_POINT ( 'NONE',  ( -62.86468353124998742, 8.973958332991934128, 1.999225269531025972 ) ) ;
#7259 = CIRCLE ( 'NONE', #10964, 1.000000000000000888 ) ;
#7260 = CARTESIAN_POINT ( 'NONE',  ( -49.99999999999998579, -15.00000000000001243, -0.1418111474832534080 ) ) ;
#7261 = ORIENTED_EDGE ( 'NONE', *, *, #10836, .T. ) ;
#7262 = CARTESIAN_POINT ( 'NONE',  ( -60.99999999999998579, 12.47916666666666607, 2.077350269189628840 ) ) ;
#7263 = CARTESIAN_POINT ( 'NONE',  ( -60.99999999999998579, 9.000000000000001776, 1.500000000000002220 ) ) ;
#7264 = CARTESIAN_POINT ( 'NONE',  ( -61.99999999999998579, 16.00000000000000000, 1.500000000000002220 ) ) ;
#7265 = AXIS2_PLACEMENT_3D ( 'NONE', #7289, #1500, #566 ) ;
#7266 = CARTESIAN_POINT ( 'NONE',  ( -61.99999999999998579, 10.15624999931720218, 2.654700538379254571 ) ) ;
#7267 = ORIENTED_EDGE ( 'NONE', *, *, #1779, .T. ) ;
#7268 = VECTOR ( 'NONE', #1565, 1000.000000000000000 ) ;
#7269 = DIRECTION ( 'NONE',  ( 1.000000000000000000, 0.000000000000000000, 0.000000000000000000 ) ) ;
#7270 = CARTESIAN_POINT ( 'NONE',  ( -61.56765823437498852, 12.53645833299193413, 2.248837904296538515 ) ) ;
#7271 = CARTESIAN_POINT ( 'NONE',  ( -61.99999999999998579, 16.00000000000000000, 2.500000000000000444 ) ) ;
#7272 = AXIS2_PLACEMENT_3D ( 'NONE', #2681, #840, #8455 ) ;
#7273 = ORIENTED_EDGE ( 'NONE', *, *, #2042, .T. ) ;
#7274 = EDGE_CURVE ( 'NONE', #2234, #767, #667, .T. ) ;
#7275 = CARTESIAN_POINT ( 'NONE',  ( -62.86468353124999453, 11.51562499965860020, 1.500000000000002220 ) ) ;
#7276 =( BOUNDED_CURVE ( )  B_SPLINE_CURVE ( 2, ( #2075, #6178, #2019, #7240, #4557, #8854, #1960, #7908, #7965 ),
 .UNSPECIFIED., .F., .T. ) 
 B_SPLINE_CURVE_WITH_KNOTS ( ( 3, 2, 2, 2, 3 ),
 ( 0.2421875000000000000, 0.2447916666666666574, 0.2500000000000000000, 0.2552083333333333148, 0.2578125000000000000 ),
 .UNSPECIFIED. ) 
 CURVE ( )  GEOMETRIC_REPRESENTATION_ITEM ( )  RATIONAL_B_SPLINE_CURVE ( ( 0.9330127018922194093, 0.9330127018922194093, 1.000000000000000000, 0.8660254037844387076, 1.000000000000000000, 0.8660254037844387076, 1.000000000000000000, 0.9330127018922194093, 0.9330127018922194093 ) ) 
 REPRESENTATION_ITEM ( '' )  );
#7277 = DIRECTION ( 'NONE',  ( 0.000000000000000000, 0.000000000000000000, -1.000000000000000000 ) ) ;
#7278 = VECTOR ( 'NONE', #1341, 1000.000000000000000 ) ;
#7279 = FACE_OUTER_BOUND ( 'NONE', #3266, .T. ) ;
#7280 = CARTESIAN_POINT ( 'NONE',  ( -61.49999999999998579, 9.458333333333332149, 2.366025403784441927 ) ) ;
#7281 = ORIENTED_EDGE ( 'NONE', *, *, #9158, .T. ) ;
#7282 = CARTESIAN_POINT ( 'NONE',  ( -62.49999999999998579, 11.16666666666666607, 2.366025403784441483 ) ) ;
#7283 = VERTEX_POINT ( 'NONE', #7504 ) ;
#7284 = UNCERTAINTY_MEASURE_WITH_UNIT (LENGTH_MEASURE( 1.000000000000000082E-05 ), #6966, 'distance_accuracy_value', 'NONE');
#7285 = CARTESIAN_POINT ( 'NONE',  ( 7.299999999999999822, 1.000000000000000000, 0.000000000000000000 ) ) ;
#7286 = CARTESIAN_POINT ( 'NONE',  ( -62.99999999999998579, 9.895833333333333925, 2.077350269189627952 ) ) ;
#7287 = VECTOR ( 'NONE', #8722, 1000.000000000000000 ) ;
#7288 = CARTESIAN_POINT ( 'NONE',  ( -62.99999999999998579, 9.572916665983870033, 0.9226497308103756012 ) ) ;
#7289 = CARTESIAN_POINT ( 'NONE',  ( -77.99999999999998579, -11.50000000000000711, 4.999999999999999112 ) ) ;
#7290 = CARTESIAN_POINT ( 'NONE',  ( -62.99999999999998579, 14.82291666598386826, 0.9226497308103756012 ) ) ;
#7291 = PRODUCT_DEFINITION_FORMATION_WITH_SPECIFIED_SOURCE ( 'ANY', '', #7422, .NOT_KNOWN. ) ;
#7292 = CARTESIAN_POINT ( 'NONE',  ( -61.99999999999998579, 11.20312499965860198, 0.5015494609379544944 ) ) ;
#7293 = ORIENTED_EDGE ( 'NONE', *, *, #10731, .T. ) ;
#7294 = CARTESIAN_POINT ( 'NONE',  ( 140.0000000000000284, 8.000000000000000000, 6.000000000000000000 ) ) ;
#7295 = EDGE_CURVE ( 'NONE', #6858, #3994, #8238, .T. ) ;
#7296 = CARTESIAN_POINT ( 'NONE',  ( -61.99999999999998579, 9.062500000000000000, 0.5000000000000013323 ) ) ;
#7297 = ORIENTED_EDGE ( 'NONE', *, *, #5886, .F. ) ;
#7298 = DIRECTION ( 'NONE',  ( -0.000000000000000000, -0.000000000000000000, -1.000000000000000000 ) ) ;
#7299 = CARTESIAN_POINT ( 'NONE',  ( -61.13531646874998415, 13.55729166632526805, 1.999225269531026417 ) ) ;
#7300 = CARTESIAN_POINT ( 'NONE',  ( -62.86468353124999453, 9.723958332991934128, 1.999225269531025750 ) ) ;
#7301 = CARTESIAN_POINT ( 'NONE',  ( -61.73205080756886076, 11.66741454900183506, 2.500000000000000000 ) ) ;
#7302 = VERTEX_POINT ( 'NONE', #625 ) ;
#7303 = FACE_OUTER_BOUND ( 'NONE', #9915, .T. ) ;
#7304 = CARTESIAN_POINT ( 'NONE',  ( -61.99999999999999289, 11.82812499965860198, 2.498450539062049724 ) ) ;
#7305 = CARTESIAN_POINT ( 'NONE',  ( -57.99999999999998579, -14.00000000000001243, 3.000000000000000000 ) ) ;
#7306 = CARTESIAN_POINT ( 'NONE',  ( -62.49999999999998579, 15.38541666598387003, 2.366025403784441483 ) ) ;
#7307 = CARTESIAN_POINT ( 'NONE',  ( -62.99999999999998579, 16.11458333265053255, 2.077350269189627952 ) ) ;
#7308 = EDGE_LOOP ( 'NONE', ( #5119, #8224, #2147, #2601 ) ) ;
#7309 = VERTEX_POINT ( 'NONE', #4005 ) ;
#7310 = VECTOR ( 'NONE', #2035, 1000.000000000000000 ) ;
#7311 = CARTESIAN_POINT ( 'NONE',  ( -61.99999999999999289, 13.39062499965860020, 0.5015494609379544944 ) ) ;
#7312 = CARTESIAN_POINT ( 'NONE',  ( -61.13531646874998415, 9.328124999658600203, 1.500000000000002220 ) ) ;
#7313 = LINE ( 'NONE', #10530, #5008 ) ;
#7314 = EDGE_LOOP ( 'NONE', ( #9312, #863, #29, #7199 ) ) ;
#7315 = CARTESIAN_POINT ( 'NONE',  ( -61.49999999999998579, 12.45833333333333393, 2.366025403784441927 ) ) ;
#7316 = CYLINDRICAL_SURFACE ( 'NONE', #5540, 0.9999999999999981126 ) ;
#7317 = FILL_AREA_STYLE ('',( #9037 ) ) ;
#7318 = CARTESIAN_POINT ( 'NONE',  ( -62.99999999999998579, 12.57291666598387003, 0.9226497308103756012 ) ) ;
#7319 = EDGE_CURVE ( 'NONE', #5402, #6260, #7922, .T. ) ;
#7320 = CARTESIAN_POINT ( 'NONE',  ( 1.299999999999999156, 0.000000000000000000, -2.000000000000000000 ) ) ;
#7321 = CARTESIAN_POINT ( 'NONE',  ( -61.99999999999998579, 12.14062499965860198, 0.5015494609379544944 ) ) ;
#7322 = CARTESIAN_POINT ( 'NONE',  ( -61.99999999999998579, 16.00000000000000000, 1.500000000000002220 ) ) ;
#7323 = ORIENTED_EDGE ( 'NONE', *, *, #1326, .T. ) ;
#7324 = CIRCLE ( 'NONE', #10698, 0.9999999999999983347 ) ;
#7325 = AXIS2_PLACEMENT_3D ( 'NONE', #9472, #1021, #3755 ) ;
#7326 = CARTESIAN_POINT ( 'NONE',  ( -61.99999999999998579, 11.07812499965860020, 2.498450539062049724 ) ) ;
#7327 = CARTESIAN_POINT ( 'NONE',  ( -61.99999999999998579, 16.00000000000000000, 1.500000000000002220 ) ) ;
#7328 = PRODUCT ( 'stationary jaw', 'stationary jaw', '', ( #5143 ) ) ;
#7329 = LINE ( 'NONE', #10820, #6193 ) ;
#7330 = ORIENTED_EDGE ( 'NONE', *, *, #4707, .F. ) ;
#7331=STYLED_ITEM('',(#11006),#1321);
#7332 = CARTESIAN_POINT ( 'NONE',  ( -76.99999999999998579, -11.50000000000000711, 5.000000000000000000 ) ) ;
#7333 = EDGE_CURVE ( 'NONE', #41, #2258, #3954, .T. ) ;
#7334 = CIRCLE ( 'NONE', #905, 1.000000000000000888 ) ;
#7335 = ORIENTED_EDGE ( 'NONE', *, *, #795, .F. ) ;
#7336 = CARTESIAN_POINT ( 'NONE',  ( -62.26794919243111082, 9.792414549001835056, 0.4999999999999982792 ) ) ;
#7337 = CARTESIAN_POINT ( 'NONE',  ( -60.99999999999998579, 10.22916666666666785, 2.077350269189628840 ) ) ;
#7338 = DIRECTION ( 'NONE',  ( -3.965082230804130220E-16, 1.000000000000000000, -0.000000000000000000 ) ) ;
#7339 = CARTESIAN_POINT ( 'NONE',  ( -61.73205080756884655, 8.198664549684629321, 2.500000000000004885 ) ) ;
#7340 = CIRCLE ( 'NONE', #2017, 1.336466033005844434 ) ;
#7341 = CARTESIAN_POINT ( 'NONE',  ( -61.99999999999998579, 15.40624999931720218, 2.500000000000002665 ) ) ;
#7342 = CARTESIAN_POINT ( 'NONE',  ( -62.86468353124998032, 11.24479166632526805, 1.000774730468978246 ) ) ;
#7343 = CARTESIAN_POINT ( 'NONE',  ( -61.06765823437498852, 8.039062499829300990, 1.500000000000002220 ) ) ;
#7344 = VERTEX_POINT ( 'NONE', #5722 ) ;
#7345 = CARTESIAN_POINT ( 'NONE',  ( -109.9999999999999289, 33.00000000000000711, 0.000000000000000000 ) ) ;
#7346 = LINE ( 'NONE', #3121, #2715 ) ;
#7347 = AXIS2_PLACEMENT_3D ( 'NONE', #10206, #6050, #7003 ) ;
#7348 = ORIENTED_EDGE ( 'NONE', *, *, #7696, .F. ) ;
#7349 = DIRECTION ( 'NONE',  ( -0.000000000000000000, -1.000000000000000000, -0.000000000000000000 ) ) ;
#7350 = CARTESIAN_POINT ( 'NONE',  ( -62.86468353124999453, 13.45312499965860020, 1.500000000000002220 ) ) ;
#7351 = CARTESIAN_POINT ( 'NONE',  ( -61.13531646874997705, 10.59895833299193413, 1.000774730468978468 ) ) ;
#7352 = CARTESIAN_POINT ( 'NONE',  ( -60.99999999999998579, 11.71874999931720218, 1.500000000000002220 ) ) ;
#7353 = ORIENTED_EDGE ( 'NONE', *, *, #2436, .F. ) ;
#7354 = CARTESIAN_POINT ( 'NONE',  ( 143.9000000000000341, -5.500000000000000000, 6.000000000000000000 ) ) ;
#7355 = CARTESIAN_POINT ( 'NONE',  ( -61.56765823437498142, 11.93229166632526805, 0.7511620957034663704 ) ) ;
#7356 = CARTESIAN_POINT ( 'NONE',  ( -61.56765823437498852, 14.84895833299193413, 2.248837904296538515 ) ) ;
#7357 = EDGE_CURVE ( 'NONE', #2734, #5709, #2337, .T. ) ;
#7358 = EDGE_CURVE ( 'NONE', #9209, #4452, #10004, .T. ) ;
#7359 = DIRECTION ( 'NONE',  ( 0.000000000000000000, -0.000000000000000000, 1.000000000000000000 ) ) ;
#7360 = CARTESIAN_POINT ( 'NONE',  ( -61.99999999999998579, 15.65624999931720218, 2.654700538379254571 ) ) ;
#7361 = DIRECTION ( 'NONE',  ( 0.000000000000000000, 0.000000000000000000, -1.000000000000000000 ) ) ;
#7362 = VERTEX_POINT ( 'NONE', #8129 ) ;
#7363 = CARTESIAN_POINT ( 'NONE',  ( 0.000000000000000000, -0.2500000000000001110, 1.312875263449798879 ) ) ;
#7364 = CARTESIAN_POINT ( 'NONE',  ( -61.99999999999998579, 16.00000000000000000, 1.500000000000002220 ) ) ;
#7365 = EDGE_CURVE ( 'NONE', #6713, #5040, #3903, .T. ) ;
#7366 = CARTESIAN_POINT ( 'NONE',  ( -61.99999999999999289, 14.76562499965860198, 2.498450539062049724 ) ) ;
#7367 = CARTESIAN_POINT ( 'NONE',  ( -62.43234176562498305, 10.41145833299193413, 0.7511620957034662593 ) ) ;
#7368 = CARTESIAN_POINT ( 'NONE',  ( -61.99999999999998579, 14.53124999931720041, 0.5000000000000013323 ) ) ;
#7369 = ORIENTED_EDGE ( 'NONE', *, *, #2448, .T. ) ;
#7370 = CARTESIAN_POINT ( 'NONE',  ( -60.99999999999998579, 14.02083333333333215, 0.9226497308103762673 ) ) ;
#7371 = EDGE_CURVE ( 'NONE', #40, #2188, #3070, .T. ) ;
#7372 = EDGE_CURVE ( 'NONE', #3431, #4466, #571, .T. ) ;
#7373 = DIRECTION ( 'NONE',  ( 0.000000000000000000, 0.000000000000000000, -1.000000000000000000 ) ) ;
#7374 =( BOUNDED_CURVE ( )  B_SPLINE_CURVE ( 2, ( #7758, #1869, #2041, #10361, #10300, #10478, #8707, #9474, #2758 ),
 .UNSPECIFIED., .F., .F. ) 
 B_SPLINE_CURVE_WITH_KNOTS ( ( 3, 2, 2, 2, 3 ),
 ( 0.3671875000000000000, 0.3697916666666666852, 0.3750000000000000000, 0.3802083333333333148, 0.3828125000000000000 ),
 .UNSPECIFIED. ) 
 CURVE ( )  GEOMETRIC_REPRESENTATION_ITEM ( )  RATIONAL_B_SPLINE_CURVE ( ( 0.9330127018922194093, 0.9330127018922194093, 1.000000000000000000, 0.8660254037844387076, 1.000000000000000000, 0.8660254037844387076, 1.000000000000000000, 0.9330127018922194093, 0.9330127018922194093 ) ) 
 REPRESENTATION_ITEM ( '' )  );
#7375 = PRESENTATION_STYLE_ASSIGNMENT (( #4135 ) ) ;
#7376 = UNCERTAINTY_MEASURE_WITH_UNIT (LENGTH_MEASURE( 1.000000000000000082E-05 ), #8986, 'distance_accuracy_value', 'NONE');
#7377 = CARTESIAN_POINT ( 'NONE',  ( -62.49999999999998579, 11.38541666598387003, 2.366025403784441483 ) ) ;
#7378 = FACE_OUTER_BOUND ( 'NONE', #5694, .T. ) ;
#7379 = CARTESIAN_POINT ( 'NONE',  ( -61.13531646874998415, 14.30729166632526983, 1.999225269531026417 ) ) ;
#7380 = CARTESIAN_POINT ( 'NONE',  ( -49.99999999999998579, -10.00000000000000888, 3.141811147483255073 ) ) ;
#7381 = EDGE_LOOP ( 'NONE', ( #5490, #5958, #870, #6768 ) ) ;
#7382 = CARTESIAN_POINT ( 'NONE',  ( -61.13531646874998415, 12.14062499965860198, 1.500000000000002220 ) ) ;
#7383 = CARTESIAN_POINT ( 'NONE',  ( -61.99999999999998579, 16.00000000000000000, 0.5000000000000041078 ) ) ;
#7384 = CARTESIAN_POINT ( 'NONE',  ( -62.86468353124999453, 15.26562499965860020, 1.500000000000002220 ) ) ;
#7385 = VERTEX_POINT ( 'NONE', #3120 ) ;
#7386 = LINE ( 'NONE', #8998, #8168 ) ;
#7387 = EDGE_CURVE ( 'NONE', #4305, #8992, #984, .T. ) ;
#7388 = EDGE_CURVE ( 'NONE', #4054, #4962, #4312, .T. ) ;
#7389 = ORIENTED_EDGE ( 'NONE', *, *, #3824, .T. ) ;
#7390 = FACE_OUTER_BOUND ( 'NONE', #4180, .T. ) ;
#7391 = CARTESIAN_POINT ( 'NONE',  ( -60.99999999999998579, 9.250000000000000000, 1.500000000000002220 ) ) ;
#7392 = CARTESIAN_POINT ( 'NONE',  ( -61.99999999999998579, 16.00000000000000000, 0.5000000000000041078 ) ) ;
#7393 = CARTESIAN_POINT ( 'NONE',  ( -61.99999999999997868, 8.437500000000000000, 2.500000000000002665 ) ) ;
#7394 = FACE_OUTER_BOUND ( 'NONE', #3706, .T. ) ;
#7395 = CARTESIAN_POINT ( 'NONE',  ( -62.99999999999998579, 8.593749999317203958, 1.500000000000001998 ) ) ;
#7396 = CARTESIAN_POINT ( 'NONE',  ( -62.43234176562498305, 12.22395833299193413, 0.7511620957034662593 ) ) ;
#7397 = DIRECTION ( 'NONE',  ( -1.000000000000000000, 0.000000000000000000, -0.000000000000000000 ) ) ;
#7398 = ORIENTED_EDGE ( 'NONE', *, *, #3167, .F. ) ;
#7399 = CARTESIAN_POINT ( 'NONE',  ( -61.49999999999998579, 9.177083332650536107, 2.366025403784441927 ) ) ;
#7400 = DIRECTION ( 'NONE',  ( -1.000000000000000000, 0.000000000000000000, 0.000000000000000000 ) ) ;
#7401 = CARTESIAN_POINT ( 'NONE',  ( -61.49999999999998579, 13.76041666598387003, 0.6339745962155628467 ) ) ;
#7402 = CARTESIAN_POINT ( 'NONE',  ( -62.86468353124998032, 13.68229166632526983, 1.000774730468978246 ) ) ;
#7403 = CARTESIAN_POINT ( 'NONE',  ( -61.49999999999998579, 13.79166666666666785, 0.6339745962155628467 ) ) ;
#7404 = CARTESIAN_POINT ( 'NONE',  ( -62.26794919243110371, 8.073664549684629321, 0.4999999999999997780 ) ) ;
#7405 = CARTESIAN_POINT ( 'NONE',  ( -62.26794919243111082, 14.17633545031537068, 2.500000000000003109 ) ) ;
#7406 = CARTESIAN_POINT ( 'NONE',  ( -61.56765823437498852, 10.84895833299193413, 2.248837904296538515 ) ) ;
#7407 = EDGE_CURVE ( 'NONE', #4570, #1925, #1668, .T. ) ;
#7408 = CARTESIAN_POINT ( 'NONE',  ( -62.86468353124999453, 15.26562499965860020, 1.500000000000002220 ) ) ;
#7409 = ITEM_DEFINED_TRANSFORMATION ( 'NONE', 'NONE', #9054,  #2307 ) ;
#7410 = LINE ( 'NONE', #7248, #5478 ) ;
#7411 = CARTESIAN_POINT ( 'NONE',  ( -62.86468353124998032, 8.494791666325268054, 1.000774730468978246 ) ) ;
#7412 = CARTESIAN_POINT ( 'NONE',  ( -105.0000000000000000, -2.500000000000000000, 3.000000000000000000 ) ) ;
#7413 = ORIENTED_EDGE ( 'NONE', *, *, #6699, .F. ) ;
#7414 = CARTESIAN_POINT ( 'NONE',  ( -62.26794919243111082, 11.89508544963257286, 2.500000000000003109 ) ) ;
#7415 = CARTESIAN_POINT ( 'NONE',  ( -61.49999999999998579, 8.041666666666667851, 0.6339745962155628467 ) ) ;
#7416 = CARTESIAN_POINT ( 'NONE',  ( -62.86468353124998032, 14.18229166632526983, 1.000774730468978024 ) ) ;
#7417 = CARTESIAN_POINT ( 'NONE',  ( -62.86468353124998742, 10.47395833299193413, 1.999225269531025972 ) ) ;
#7418 = CONICAL_SURFACE ( 'NONE', #1546, 1.886264737416298631, 0.08726646259971662656 ) ;
#7419 = DIRECTION ( 'NONE',  ( -1.000000000000000000, 0.000000000000000000, -0.000000000000000000 ) ) ;
#7420 = EDGE_LOOP ( 'NONE', ( #8853, #6324, #9218, #10203 ) ) ;
#7421 = CARTESIAN_POINT ( 'NONE',  ( -61.99999999999998579, 13.18750000000000000, 2.654700538379254571 ) ) ;
#7422 = PRODUCT ( 'fine adjustment wheel', 'fine adjustment wheel', '', ( #8973 ) ) ;
#7423 = CARTESIAN_POINT ( 'NONE',  ( -62.49999999999998579, 11.13541666598387003, 2.366025403784441483 ) ) ;
#7424 = ADVANCED_FACE ( 'NONE', ( #931 ), #9378, .T. ) ;
#7425 =( NAMED_UNIT ( * ) SI_UNIT ( $, .STERADIAN. ) SOLID_ANGLE_UNIT ( ) );
#7426 = CARTESIAN_POINT ( 'NONE',  ( -62.49999999999998579, 12.13541666598386826, 2.366025403784441483 ) ) ;
#7427 = AXIS2_PLACEMENT_3D ( 'NONE', #5781, #631, #1412 ) ;
#7428 = ADVANCED_FACE ( 'NONE', ( #3377 ), #8493, .F. ) ;
#7429 = ADVANCED_FACE ( 'NONE', ( #10257 ), #9323, .F. ) ;
#7430 = VECTOR ( 'NONE', #6110, 1000.000000000000000 ) ;
#7431 = CARTESIAN_POINT ( 'NONE',  ( -61.56765823437498142, 13.61979166632526805, 0.7511620957034663704 ) ) ;
#7432 = CYLINDRICAL_SURFACE ( 'NONE', #9191, 0.9999999999999981126 ) ;
#7433 =( BOUNDED_CURVE ( )  B_SPLINE_CURVE ( 2, ( #4914, #10865, #3202, #7537, #1535, #10715, #4970, #705, #10915 ),
 .UNSPECIFIED., .F., .F. ) 
 B_SPLINE_CURVE_WITH_KNOTS ( ( 3, 2, 2, 2, 3 ),
 ( 0.4296875000000000555, 0.4322916666666666852, 0.4375000000000000000, 0.4427083333333333148, 0.4453125000000000000 ),
 .UNSPECIFIED. ) 
 CURVE ( )  GEOMETRIC_REPRESENTATION_ITEM ( )  RATIONAL_B_SPLINE_CURVE ( ( 0.9330127018922192983, 0.9330127018922207416, 1.000000000000000000, 0.8660254037844387076, 1.000000000000000000, 0.8660254037844387076, 1.000000000000000000, 0.9330127018922194093, 0.9330127018922194093 ) ) 
 REPRESENTATION_ITEM ( '' )  );
#7434 = VERTEX_POINT ( 'NONE', #5937 ) ;
#7435 = VECTOR ( 'NONE', #7229, 999.9999999999998863 ) ;
#7436 = CARTESIAN_POINT ( 'NONE',  ( -61.99999999999998579, 11.70312499965860020, 0.5015494609379544944 ) ) ;
#7437 = FACE_OUTER_BOUND ( 'NONE', #7879, .T. ) ;
#7438 = CARTESIAN_POINT ( 'NONE',  ( -61.13531646874998415, 15.86979166632526628, 1.999225269531026417 ) ) ;
#7439 = ORIENTED_EDGE ( 'NONE', *, *, #3764, .T. ) ;
#7440 = LINE ( 'NONE', #7332, #6752 ) ;
#7441 = VECTOR ( 'NONE', #6000, 1000.000000000000000 ) ;
#7442 = MECHANICAL_DESIGN_GEOMETRIC_PRESENTATION_REPRESENTATION (  '', ( #4234 ), #2125 ) ;
#7443 = ORIENTED_EDGE ( 'NONE', *, *, #5823, .T. ) ;
#7444 = CARTESIAN_POINT ( 'NONE',  ( -60.99999999999998579, 8.718749999317203958, 1.500000000000002220 ) ) ;
#7445 = CARTESIAN_POINT ( 'NONE',  ( -61.99999999999998579, 9.187500000000000000, 2.654700538379254571 ) ) ;
#7446 = CARTESIAN_POINT ( 'NONE',  ( -62.86468353124998032, 8.244791666325268054, 1.000774730468978246 ) ) ;
#7447 = CARTESIAN_POINT ( 'NONE',  ( -60.99999999999998579, 8.250000000000000000, 1.500000000000002220 ) ) ;
#7448 = AXIS2_PLACEMENT_3D ( 'NONE', #6661, #88, #2420 ) ;
#7449 = CARTESIAN_POINT ( 'NONE',  ( -61.73205080756886076, 15.52008544963257108, 0.5000000000000014433 ) ) ;
#7450 = CARTESIAN_POINT ( 'NONE',  ( -62.43234176562499016, 11.80729166632526805, 2.248837904296538071 ) ) ;
#7451 = EDGE_CURVE ( 'NONE', #3127, #9814, #9433, .T. ) ;
#7452 = COLOUR_RGB ( '',0.8941176470588234615, 0.8941176470588234615, 0.8941176470588234615 ) ;
#7453 = CARTESIAN_POINT ( 'NONE',  ( -62.26794919243111082, 10.57366454968463110, 0.5000000000000013323 ) ) ;
#7454 = ORIENTED_EDGE ( 'NONE', *, *, #10783, .F. ) ;
#7455 = CARTESIAN_POINT ( 'NONE',  ( 150.0000000000000284, -8.000000000000000000, 0.000000000000000000 ) ) ;
#7456 = CIRCLE ( 'NONE', #1250, 1.000000000000000888 ) ;
#7457 = CARTESIAN_POINT ( 'NONE',  ( -49.99998799999998766, 0.000000000000000000, -0.1418111474832477736 ) ) ;
#7458 = CARTESIAN_POINT ( 'NONE',  ( -61.13531646874998415, 13.80729166632526983, 1.999225269531026417 ) ) ;
#7459 = CARTESIAN_POINT ( 'NONE',  ( -120.0000000000000000, 15.67949192431120053, 83.15773105863907233 ) ) ;
#7460 = PRODUCT_DEFINITION_FORMATION_WITH_SPECIFIED_SOURCE ( 'ANY', '', #48, .NOT_KNOWN. ) ;
#7461 = CARTESIAN_POINT ( 'NONE',  ( -62.49999999999998579, 8.083333333333332149, 0.6339745962155627357 ) ) ;
#7462 = DIRECTION ( 'NONE',  ( -1.000000000000000000, 0.000000000000000000, 0.000000000000000000 ) ) ;
#7463 = CARTESIAN_POINT ( 'NONE',  ( -62.86468353124998032, 12.24479166632526805, 1.000774730468978024 ) ) ;
#7464 = CARTESIAN_POINT ( 'NONE',  ( -62.43234176562499016, 15.05729166632526805, 2.248837904296538071 ) ) ;
#7465 = CARTESIAN_POINT ( 'NONE',  ( -76.89999999999999147, 11.49999999999999645, -2.000000000000001332 ) ) ;
#7466 = CONTEXT_DEPENDENT_SHAPE_REPRESENTATION ( #1087, #3417 ) ;
#7467 = DIRECTION ( 'NONE',  ( -0.000000000000000000, -1.000000000000000000, -0.000000000000000000 ) ) ;
#7468 = CARTESIAN_POINT ( 'NONE',  ( -61.56765823437498142, 8.182291666325268054, 0.7511620957034663704 ) ) ;
#7469 = DIRECTION ( 'NONE',  ( -0.000000000000000000, -1.000000000000000000, -0.000000000000000000 ) ) ;
#7470 = ORIENTED_EDGE ( 'NONE', *, *, #6688, .F. ) ;
#7471 = FACE_OUTER_BOUND ( 'NONE', #409, .T. ) ;
#7472 = DIRECTION ( 'NONE',  ( 0.000000000000000000, 0.000000000000000000, -1.000000000000000000 ) ) ;
#7473 = EDGE_CURVE ( 'NONE', #10538, #1136, #6398, .T. ) ;
#7474 = CARTESIAN_POINT ( 'NONE',  ( -62.43234176562498305, 13.91145833299193413, 0.7511620957034662593 ) ) ;
#7475 = CARTESIAN_POINT ( 'NONE',  ( -62.43234176562498305, 9.911458332991934128, 0.7511620957034662593 ) ) ;
#7476 = CARTESIAN_POINT ( 'NONE',  ( -61.13531646874997705, 8.098958332991934128, 1.000774730468978468 ) ) ;
#7477 = CARTESIAN_POINT ( 'NONE',  ( -61.73205080756886076, 14.52008544963257286, 0.5000000000000014433 ) ) ;
#7478 = VERTEX_POINT ( 'NONE', #8439 ) ;
#7479 = CARTESIAN_POINT ( 'NONE',  ( -60.99999999999998579, 13.77083333333333215, 0.9226497308103762673 ) ) ;
#7480 = CARTESIAN_POINT ( 'NONE',  ( -62.43234176562499016, 9.307291666325268054, 2.248837904296538071 ) ) ;
#7481 =( NAMED_UNIT ( * ) PLANE_ANGLE_UNIT ( ) SI_UNIT ( $, .RADIAN. ) );
#7482 = CARTESIAN_POINT ( 'NONE',  ( -62.49999999999998579, 11.80208333265053611, 0.6339745962155627357 ) ) ;
#7483 = CARTESIAN_POINT ( 'NONE',  ( -62.86468353124999453, 14.45312499965860020, 1.500000000000002220 ) ) ;
#7484 = DIRECTION ( 'NONE',  ( 0.000000000000000000, 0.000000000000000000, -1.000000000000000000 ) ) ;
#7485 = ORIENTED_EDGE ( 'NONE', *, *, #7867, .T. ) ;
#7486 = CARTESIAN_POINT ( 'NONE',  ( -61.99999999999998579, 12.20312499965860198, 0.5015494609379544944 ) ) ;
#7487 = CARTESIAN_POINT ( 'NONE',  ( -61.99999999999998579, 16.00000000000000000, 1.500000000000002220 ) ) ;
#7488 = DIRECTION ( 'NONE',  ( 1.000000000000000000, 0.000000000000000000, 0.000000000000000000 ) ) ;
#7489 = ORIENTED_EDGE ( 'NONE', *, *, #10310, .T. ) ;
#7490 = DIRECTION ( 'NONE',  ( 0.000000000000000000, 0.000000000000000000, 1.000000000000000000 ) ) ;
#7491 =( BOUNDED_CURVE ( )  B_SPLINE_CURVE ( 2, ( #1246, #239, #3624, #675, #9074, #3912, #4060, #7405, #579 ),
 .UNSPECIFIED., .F., .F. ) 
 B_SPLINE_CURVE_WITH_KNOTS ( ( 3, 2, 2, 2, 3 ),
 ( 0.7578125000000000000, 0.7604166666666666297, 0.7656250000000000000, 0.7708333333333333703, 0.7734375000000000000 ),
 .UNSPECIFIED. ) 
 CURVE ( )  GEOMETRIC_REPRESENTATION_ITEM ( )  RATIONAL_B_SPLINE_CURVE ( ( 0.9330127018922194093, 0.9330127018922194093, 1.000000000000000000, 0.8660254037844387076, 1.000000000000000000, 0.8660254037844387076, 1.000000000000000000, 0.9330127018922194093, 0.9330127018922194093 ) ) 
 REPRESENTATION_ITEM ( '' )  );
#7492 = AXIS2_PLACEMENT_3D ( 'NONE', #2472, #5120, #10809 ) ;
#7493 = VERTEX_POINT ( 'NONE', #2666 ) ;
#7494 = DIRECTION ( 'NONE',  ( -1.000000000000000000, 0.000000000000000000, 0.000000000000000000 ) ) ;
#7495 = CARTESIAN_POINT ( 'NONE',  ( -61.49999999999998579, 11.54166666666666785, 0.6339745962155628467 ) ) ;
#7496 = CARTESIAN_POINT ( 'NONE',  ( -49.99999999999998579, 14.99999999999998579, 83.15773105863907233 ) ) ;
#7497 = CARTESIAN_POINT ( 'NONE',  ( -149.9999999999999716, 8.000000000000000000, 3.000000000000000000 ) ) ;
#7498 = ADVANCED_FACE ( 'NONE', ( #158, #2602 ), #8390, .F. ) ;
#7499 = CARTESIAN_POINT ( 'NONE',  ( -61.99999999999998579, 9.656249999317200405, 2.654700538379254571 ) ) ;
#7500 = AXIS2_PLACEMENT_3D ( 'NONE', #9070, #7298, #3073 ) ;
#7501 = CARTESIAN_POINT ( 'NONE',  ( -61.13531646874998415, 13.64062499965860198, 1.500000000000002220 ) ) ;
#7502 = CARTESIAN_POINT ( 'NONE',  ( -62.49999999999998579, 10.66666666666666607, 2.366025403784441483 ) ) ;
#7503 = ORIENTED_EDGE ( 'NONE', *, *, #9500, .T. ) ;
#7504 = CARTESIAN_POINT ( 'NONE',  ( -144.9999999999999716, 33.00000000000000000, 3.000000000000000000 ) ) ;
#7505 = PRODUCT_DEFINITION_SHAPE ( 'NONE', 'NONE',  #10992 ) ;
#7506 = ORIENTED_EDGE ( 'NONE', *, *, #741, .F. ) ;
#7507 = LINE ( 'NONE', #6471, #4472 ) ;
#7508 = CARTESIAN_POINT ( 'NONE',  ( -62.86468353124998742, 14.72395833299193413, 1.999225269531025972 ) ) ;
#7509 = CARTESIAN_POINT ( 'NONE',  ( -61.73205080756886076, 13.69866454968463110, 2.500000000000003109 ) ) ;
#7510 = CARTESIAN_POINT ( 'NONE',  ( 143.9000000000000341, -5.500000000000000000, 3.000000000000000888 ) ) ;
#7511 = CARTESIAN_POINT ( 'NONE',  ( -61.99999999999998579, 16.00000000000000000, 1.500000000000002220 ) ) ;
#7512 = CARTESIAN_POINT ( 'NONE',  ( -61.56765823437498142, 12.18229166632526628, 0.7511620957034663704 ) ) ;
#7513 = CARTESIAN_POINT ( 'NONE',  ( -61.56765823437498852, 16.09895833299193768, 2.248837904296538515 ) ) ;
#7514 = DIRECTION ( 'NONE',  ( -0.8571673013836855759, 0.000000000000000000, -0.5150380737757257466 ) ) ;
#7515 = CYLINDRICAL_SURFACE ( 'NONE', #10807, 0.9999999999999981126 ) ;
#7516 = CARTESIAN_POINT ( 'NONE',  ( -60.99999999999998579, 16.19791666598386826, 2.077350269189628840 ) ) ;
#7517 = CARTESIAN_POINT ( 'NONE',  ( -49.99999999999998579, 14.99999999999998579, -2.000000000000000000 ) ) ;
#7518 = ORIENTED_EDGE ( 'NONE', *, *, #3408, .T. ) ;
#7519 = VECTOR ( 'NONE', #2279, 999.9999999999998863 ) ;
#7520 = CARTESIAN_POINT ( 'NONE',  ( -62.99999999999998579, 11.84374999931720218, 1.500000000000001998 ) ) ;
#7521 = CARTESIAN_POINT ( 'NONE',  ( -60.99999999999998579, 8.020833333333332149, 0.9226497308103762673 ) ) ;
#7522 = EDGE_CURVE ( 'NONE', #5087, #35, #3542, .T. ) ;
#7523 = CARTESIAN_POINT ( 'NONE',  ( -61.13531646874997705, 14.55729166632526983, 1.999225269531026417 ) ) ;
#7524 = CARTESIAN_POINT ( 'NONE',  ( -61.56765823437498852, 9.536458332991934128, 2.248837904296538515 ) ) ;
#7525 = EDGE_CURVE ( 'NONE', #8694, #3964, #6780, .T. ) ;
#7526 = CARTESIAN_POINT ( 'NONE',  ( -61.13531646874998415, 15.39062499965860020, 1.500000000000002220 ) ) ;
#7527 = CARTESIAN_POINT ( 'NONE',  ( -61.99999999999998579, 8.781249999317202182, 0.5000000000000013323 ) ) ;
#7528 = ORIENTED_EDGE ( 'NONE', *, *, #7165, .F. ) ;
#7529 = CARTESIAN_POINT ( 'NONE',  ( -62.99999999999998579, 13.10416666666666607, 0.9226497308103756012 ) ) ;
#7530 = CARTESIAN_POINT ( 'NONE',  ( -61.99999999999999289, 8.328124999658601979, 2.498450539062049724 ) ) ;
#7531 = SURFACE_STYLE_FILL_AREA ( #4081 ) ;
#7532 = ADVANCED_FACE ( 'NONE', ( #7555 ), #10819, .T. ) ;
#7533 = CARTESIAN_POINT ( 'NONE',  ( -62.99999999999998579, 11.82291666598387003, 0.9226497308103756012 ) ) ;
#7534 = CARTESIAN_POINT ( 'NONE',  ( -61.99999999999998579, 11.28124999931720041, 0.5000000000000013323 ) ) ;
#7535 = PRODUCT_RELATED_PRODUCT_CATEGORY ( 'part', '', ( #6542 ) ) ;
#7536 = CARTESIAN_POINT ( 'NONE',  ( -61.13531646874998415, 14.32812499965860020, 1.500000000000002220 ) ) ;
#7537 = CARTESIAN_POINT ( 'NONE',  ( -60.99999999999998579, 11.47916666666666785, 2.077350269189628840 ) ) ;
#7538 = VERTEX_POINT ( 'NONE', #5986 ) ;
#7539 = CARTESIAN_POINT ( 'NONE',  ( -62.43234176562499016, 13.30729166632526805, 2.248837904296538071 ) ) ;
#7540 = LINE ( 'NONE', #3309, #4587 ) ;
#7541 = EDGE_CURVE ( 'NONE', #6239, #4238, #6364, .T. ) ;
#7542 = CARTESIAN_POINT ( 'NONE',  ( -42.47213595499957961, -18.00000000000001066, 0.000000000000000000 ) ) ;
#7543 = ORIENTED_EDGE ( 'NONE', *, *, #9274, .F. ) ;
#7544 = CARTESIAN_POINT ( 'NONE',  ( 190.0000000000000000, -6.123233995736783046E-16, 4.000000000000000000 ) ) ;
#7545 = EDGE_LOOP ( 'NONE', ( #4428, #7625, #3209, #3933 ) ) ;
#7546 = CARTESIAN_POINT ( 'NONE',  ( -62.99999999999998579, 11.62500000000000000, 1.500000000000001998 ) ) ;
#7547 = ORIENTED_EDGE ( 'NONE', *, *, #10541, .F. ) ;
#7548 = CARTESIAN_POINT ( 'NONE',  ( -61.13531646874998415, 8.619791666325268054, 1.999225269531026417 ) ) ;
#7549 = CARTESIAN_POINT ( 'NONE',  ( -61.99999999999998579, 26.00000000000000355, 4.000000000000004441 ) ) ;
#7550 = EDGE_CURVE ( 'NONE', #1260, #6004, #5202, .T. ) ;
#7551 = CARTESIAN_POINT ( 'NONE',  ( -61.13531646874998415, 12.89062499965860198, 1.500000000000002220 ) ) ;
#7552 = CARTESIAN_POINT ( 'NONE',  ( -62.99999999999998579, 14.57291666598387003, 0.9226497308103756012 ) ) ;
#7553 = ORIENTED_EDGE ( 'NONE', *, *, #7388, .T. ) ;
#7554 =( BOUNDED_CURVE ( )  B_SPLINE_CURVE ( 2, ( #6311, #4739, #8035, #9751, #5521 ),
 .UNSPECIFIED., .F., .T. ) 
 B_SPLINE_CURVE_WITH_KNOTS ( ( 3, 2, 3 ),
 ( 0.9725886266600324292, 0.9739583333333333703, 0.9765625000000000000 ),
 .UNSPECIFIED. ) 
 CURVE ( )  GEOMETRIC_REPRESENTATION_ITEM ( )  RATIONAL_B_SPLINE_CURVE ( ( 0.9480652127606670199, 0.9647668674900635732, 1.000000000000000000, 0.9330127018922194093, 0.9330127018922194093 ) ) 
 REPRESENTATION_ITEM ( '' )  );
#7555 = FACE_OUTER_BOUND ( 'NONE', #461, .T. ) ;
#7556 = ADVANCED_FACE ( 'NONE', ( #1279 ), #5428, .T. ) ;
#7557 = VERTEX_POINT ( 'NONE', #2055 ) ;
#7558 = CARTESIAN_POINT ( 'NONE',  ( -49.99999999999998579, -15.00000000000001066, 3.000000000000000000 ) ) ;
#7559 = CARTESIAN_POINT ( 'NONE',  ( -62.43234176562499016, 15.24479166632526805, 2.248837904296538071 ) ) ;
#7560 = CARTESIAN_POINT ( 'NONE',  ( -61.99999999999998579, 11.93750000000000000, 2.500000000000002665 ) ) ;
#7561 = CARTESIAN_POINT ( 'NONE',  ( -60.99999999999998579, 11.73958333265053611, 0.9226497308103762673 ) ) ;
#7562 = FACE_OUTER_BOUND ( 'NONE', #8424, .T. ) ;
#7563 = CARTESIAN_POINT ( 'NONE',  ( -61.56765823437498852, 12.84895833299193413, 2.248837904296538515 ) ) ;
#7564 = CARTESIAN_POINT ( 'NONE',  ( -62.86468353124998742, 15.28645833299193413, 1.999225269531025972 ) ) ;
#7565 = CARTESIAN_POINT ( 'NONE',  ( 195.0000000000000000, 0.000000000000000000, 4.000000000000000000 ) ) ;
#7566 = CARTESIAN_POINT ( 'NONE',  ( -120.0000000000000000, -8.000000000000000000, -2.000000000000000000 ) ) ;
#7567 = CARTESIAN_POINT ( 'NONE',  ( -61.99999999999998579, 9.078124999658601979, 2.498450539062049724 ) ) ;
#7568 = CYLINDRICAL_SURFACE ( 'NONE', #9093, 0.9999999999999981126 ) ;
#7569 = EDGE_LOOP ( 'NONE', ( #587, #1141, #4523, #5790, #2495, #8793 ) ) ;
#7570 = DIRECTION ( 'NONE',  ( 0.000000000000000000, -1.224646799147352961E-16, 1.000000000000000000 ) ) ;
#7571 = FACE_OUTER_BOUND ( 'NONE', #7215, .T. ) ;
#7572 = CARTESIAN_POINT ( 'NONE',  ( -62.86468353124999453, 14.72395833299193413, 1.999225269531025750 ) ) ;
#7573 = CARTESIAN_POINT ( 'NONE',  ( -61.99999999999998579, 11.01562499965859843, 2.498450539062049724 ) ) ;
#7574 = CARTESIAN_POINT ( 'NONE',  ( -61.99999999999999289, 15.57812499965860198, 2.498450539062049724 ) ) ;
#7575 = DIRECTION ( 'NONE',  ( -0.000000000000000000, -0.000000000000000000, -1.000000000000000000 ) ) ;
#7576 = ORIENTED_EDGE ( 'NONE', *, *, #5198, .T. ) ;
#7577 = CARTESIAN_POINT ( 'NONE',  ( -62.49999999999998579, 14.83333333333333393, 0.6339745962155627357 ) ) ;
#7578 = CARTESIAN_POINT ( 'NONE',  ( -61.56765823437498852, 8.348958332991934128, 2.248837904296538515 ) ) ;
#7579 = FILL_AREA_STYLE ('',( #3146 ) ) ;
#7580 = EDGE_CURVE ( 'NONE', #4783, #1578, #5312, .T. ) ;
#7581 = CARTESIAN_POINT ( 'NONE',  ( -62.49999999999998579, 13.13541666598387003, 2.366025403784441483 ) ) ;
#7582 = ORIENTED_EDGE ( 'NONE', *, *, #2371, .F. ) ;
#7583 = CARTESIAN_POINT ( 'NONE',  ( -61.99999999999998579, 16.00000000000000000, 1.500000000000002220 ) ) ;
#7584 = EDGE_CURVE ( 'NONE', #1707, #6709, #4601, .T. ) ;
#7585 = AXIS2_PLACEMENT_3D ( 'NONE', #7821, #7040, #7936 ) ;
#7586 = CARTESIAN_POINT ( 'NONE',  ( -62.43234176562498305, 14.16145833299193413, 0.7511620957034662593 ) ) ;
#7587 = ORIENTED_EDGE ( 'NONE', *, *, #5031, .T. ) ;
#7588 = DIRECTION ( 'NONE',  ( -0.000000000000000000, 0.000000000000000000, -1.000000000000000000 ) ) ;
#7589 = CARTESIAN_POINT ( 'NONE',  ( -61.99999999999998579, 13.57812499965860020, 2.498450539062049724 ) ) ;
#7590 = FACE_OUTER_BOUND ( 'NONE', #1278, .T. ) ;
#7591 = AXIS2_PLACEMENT_3D ( 'NONE', #6476, #10009, #6679 ) ;
#7592 = EDGE_LOOP ( 'NONE', ( #9407, #6197, #4123, #5146 ) ) ;
#7593 = PRODUCT ( 'clamp screw', 'clamp screw', '', ( #9688 ) ) ;
#7594 = CARTESIAN_POINT ( 'NONE',  ( 0.5999999999999999778, 0.000000000000000000, 0.000000000000000000 ) ) ;
#7595 = ORIENTED_EDGE ( 'NONE', *, *, #6688, .T. ) ;
#7596 = DIRECTION ( 'NONE',  ( -0.000000000000000000, 0.000000000000000000, 1.000000000000000000 ) ) ;
#7597 = EDGE_CURVE ( 'NONE', #1245, #7701, #9488, .T. ) ;
#7598 = VECTOR ( 'NONE', #220, 1000.000000000000000 ) ;
#7599 = EDGE_LOOP ( 'NONE', ( #789, #10703, #8237, #2490, #4326, #8660 ) ) ;
#7600 = CARTESIAN_POINT ( 'NONE',  ( -61.49999999999998579, 11.70833333333333215, 2.366025403784441927 ) ) ;
#7601 = ORIENTED_EDGE ( 'NONE', *, *, #1495, .F. ) ;
#7602 = VECTOR ( 'NONE', #3708, 1000.000000000000000 ) ;
#7603 = CARTESIAN_POINT ( 'NONE',  ( -62.86468353124999453, 8.765624999658601979, 1.500000000000002220 ) ) ;
#7604 = DIRECTION ( 'NONE',  ( 0.000000000000000000, -0.000000000000000000, -1.000000000000000000 ) ) ;
#7605 = AXIS2_PLACEMENT_3D ( 'NONE', #6171, #4440, #7124 ) ;
#7606 = CARTESIAN_POINT ( 'NONE',  ( -61.13531646874998415, 13.11979166632526805, 1.999225269531026417 ) ) ;
#7607 = CARTESIAN_POINT ( 'NONE',  ( -62.26794919243111082, 9.395085449632572860, 2.500000000000000888 ) ) ;
#7608 = ORIENTED_EDGE ( 'NONE', *, *, #10027, .F. ) ;
#7609 = CARTESIAN_POINT ( 'NONE',  ( -61.99999999999997868, 10.90624999931720218, 2.500000000000002665 ) ) ;
#7610 = AXIS2_PLACEMENT_3D ( 'NONE', #7327, #2220, #3205 ) ;
#7611 = FACE_OUTER_BOUND ( 'NONE', #9630, .T. ) ;
#7612 = CARTESIAN_POINT ( 'NONE',  ( -61.99999999999998579, 13.28124999931720041, 0.5000000000000013323 ) ) ;
#7613 = CARTESIAN_POINT ( 'NONE',  ( -61.56765823437498852, 15.28645833299193590, 2.248837904296538515 ) ) ;
#7614 = VECTOR ( 'NONE', #4897, 1000.000000000000000 ) ;
#7615 = CARTESIAN_POINT ( 'NONE',  ( -62.26794919243111082, 11.92633545031536890, 2.500000000000003109 ) ) ;
#7616 = FACE_OUTER_BOUND ( 'NONE', #6346, .T. ) ;
#7617 = CARTESIAN_POINT ( 'NONE',  ( -61.49999999999998579, 10.70833333333333393, 2.366025403784441927 ) ) ;
#7618 = CARTESIAN_POINT ( 'NONE',  ( -62.86468353124998032, 12.99479166632526805, 1.000774730468978024 ) ) ;
#7619 = CARTESIAN_POINT ( 'NONE',  ( -61.13531646874998415, 9.348958332991935904, 1.000774730468978468 ) ) ;
#7620 = FACE_OUTER_BOUND ( 'NONE', #8539, .T. ) ;
#7621 =( BOUNDED_CURVE ( )  B_SPLINE_CURVE ( 2, ( #5171, #8633, #7694, #3401, #75, #1071, #958, #1012, #4459 ),
 .UNSPECIFIED., .F., .T. ) 
 B_SPLINE_CURVE_WITH_KNOTS ( ( 3, 2, 2, 2, 3 ),
 ( 0.6328125000000000000, 0.6354166666666666297, 0.6406250000000000000, 0.6458333333333333703, 0.6484375000000000000 ),
 .UNSPECIFIED. ) 
 CURVE ( )  GEOMETRIC_REPRESENTATION_ITEM ( )  RATIONAL_B_SPLINE_CURVE ( ( 0.9330127018922194093, 0.9330127018922194093, 1.000000000000000000, 0.8660254037844387076, 1.000000000000000000, 0.8660254037844387076, 1.000000000000000000, 0.9330127018922194093, 0.9330127018922194093 ) ) 
 REPRESENTATION_ITEM ( '' )  );
#7622 = CARTESIAN_POINT ( 'NONE',  ( -61.99999999999998579, 9.406249999317202182, 2.500000000000002665 ) ) ;
#7623 = CARTESIAN_POINT ( 'NONE',  ( -62.86468353124999453, 8.765624999658601979, 1.500000000000002220 ) ) ;
#7624 = DIRECTION ( 'NONE',  ( 0.000000000000000000, -0.000000000000000000, 1.000000000000000000 ) ) ;
#7625 = ORIENTED_EDGE ( 'NONE', *, *, #964, .T. ) ;
#7626 = DIRECTION ( 'NONE',  ( -0.000000000000000000, -1.000000000000000000, -0.000000000000000000 ) ) ;
#7627 = DIRECTION ( 'NONE',  ( -1.000000000000000000, -0.000000000000000000, -0.000000000000000000 ) ) ;
#7628 = CONICAL_SURFACE ( 'NONE', #8176, 1.886264737416298631, 0.08726646259971662656 ) ;
#7629 = CARTESIAN_POINT ( 'NONE',  ( -62.43234176562499016, 15.49479166632526628, 2.248837904296538071 ) ) ;
#7630 = CARTESIAN_POINT ( 'NONE',  ( -61.56765823437498852, 10.78645833299193413, 2.248837904296538515 ) ) ;
#7631 = CARTESIAN_POINT ( 'NONE',  ( -62.86468353124999453, 15.76562499965860198, 1.500000000000002220 ) ) ;
#7632 = CARTESIAN_POINT ( 'NONE',  ( -61.99999999999997868, 9.656249999317202182, 2.500000000000002665 ) ) ;
#7633 = ORIENTED_EDGE ( 'NONE', *, *, #8375, .T. ) ;
#7634 = CARTESIAN_POINT ( 'NONE',  ( -61.49999999999998579, 14.70833333333333393, 2.366025403784441927 ) ) ;
#7635 = CARTESIAN_POINT ( 'NONE',  ( 0.6000000000000000888, 0.000000000000000000, 0.000000000000000000 ) ) ;
#7636 = VECTOR ( 'NONE', #3421, 1000.000000000000000 ) ;
#7637 =( NAMED_UNIT ( * ) SI_UNIT ( $, .STERADIAN. ) SOLID_ANGLE_UNIT ( ) );
#7638 = EDGE_CURVE ( 'NONE', #10242, #8297, #10654, .T. ) ;
#7639 = CARTESIAN_POINT ( 'NONE',  ( -61.99999999999998579, 13.90624999931720218, 2.654700538379254571 ) ) ;
#7640 = ORIENTED_EDGE ( 'NONE', *, *, #7295, .T. ) ;
#7641 = SURFACE_STYLE_USAGE ( .BOTH. , #4181 ) ;
#7642 = CARTESIAN_POINT ( 'NONE',  ( -61.13531646874997705, 11.09895833299193590, 1.000774730468978468 ) ) ;
#7643 = CARTESIAN_POINT ( 'NONE',  ( 145.0000000000000284, 5.500000000000000000, 3.000000000000000000 ) ) ;
#7644 = ORIENTED_EDGE ( 'NONE', *, *, #4417, .F. ) ;
#7645 = LINE ( 'NONE', #135, #1324 ) ;
#7646 = ADVANCED_FACE ( 'NONE', ( #6335 ), #7113, .T. ) ;
#7647 = CARTESIAN_POINT ( 'NONE',  ( -61.56765823437498852, 12.84895833299193413, 2.248837904296538515 ) ) ;
#7648 = CARTESIAN_POINT ( 'NONE',  ( -109.9999999999999289, 33.00000000000000711, -2.000000000000000000 ) ) ;
#7649 = ORIENTED_EDGE ( 'NONE', *, *, #3757, .T. ) ;
#7650 = DIRECTION ( 'NONE',  ( 1.000000000000000000, 1.224646799147355672E-16, 0.000000000000000000 ) ) ;
#7651 = ORIENTED_EDGE ( 'NONE', *, *, #9211, .F. ) ;
#7652 = CARTESIAN_POINT ( 'NONE',  ( 0.5999999999999999778, 0.000000000000000000, 1.336466033005844434 ) ) ;
#7653 = PRESENTATION_STYLE_ASSIGNMENT (( #1876 ) ) ;
#7654 = ORIENTED_EDGE ( 'NONE', *, *, #1614, .F. ) ;
#7655 = VECTOR ( 'NONE', #6803, 1000.000000000000000 ) ;
#7656 = EDGE_LOOP ( 'NONE', ( #10033, #2653, #4855, #10245, #2962, #2290, #9401, #8018 ) ) ;
#7657 = CARTESIAN_POINT ( 'NONE',  ( -61.13531646874998415, 8.390624999658601979, 1.500000000000002220 ) ) ;
#7658 = CARTESIAN_POINT ( 'NONE',  ( -60.99999999999998579, 14.27083333333333393, 0.9226497308103762673 ) ) ;
#7659 = CONTEXT_DEPENDENT_SHAPE_REPRESENTATION ( #9458, #7505 ) ;
#7660 = EDGE_CURVE ( 'NONE', #7344, #6810, #10602, .T. ) ;
#7661 = CARTESIAN_POINT ( 'NONE',  ( -62.43234176562498305, 13.47395833299193413, 0.7511620957034662593 ) ) ;
#7662 = CARTESIAN_POINT ( 'NONE',  ( -149.9999999999999716, -8.000000000000000000, 0.000000000000000000 ) ) ;
#7663 = ORIENTED_EDGE ( 'NONE', *, *, #6789, .T. ) ;
#7664 = AXIS2_PLACEMENT_3D ( 'NONE', #737, #1521, #5738 ) ;
#7665 = CARTESIAN_POINT ( 'NONE',  ( -61.99999999999998579, 16.00000000000000000, 2.500000000000000444 ) ) ;
#7666 = PRODUCT_RELATED_PRODUCT_CATEGORY ( 'part', '', ( #7422 ) ) ;
#7667 = VERTEX_POINT ( 'NONE', #1040 ) ;
#7668 = CARTESIAN_POINT ( 'NONE',  ( -61.73205080756886076, 13.16741454900183328, 2.500000000000003109 ) ) ;
#7669 = CARTESIAN_POINT ( 'NONE',  ( -61.99999999999998579, 15.51562499965860198, 2.498450539062049724 ) ) ;
#7670 = CARTESIAN_POINT ( 'NONE',  ( -144.9999999999999432, 8.000000000000000000, 3.000000000000000000 ) ) ;
#7671 = DIRECTION ( 'NONE',  ( -0.000000000000000000, -1.000000000000000000, -0.000000000000000000 ) ) ;
#7672 = CARTESIAN_POINT ( 'NONE',  ( -62.49999999999998579, 8.833333333333333925, 0.6339745962155627357 ) ) ;
#7673 = VECTOR ( 'NONE', #2771, 1000.000000000000000 ) ;
#7674 = CARTESIAN_POINT ( 'NONE',  ( -62.86468353124999453, 12.26562499965860198, 1.500000000000002220 ) ) ;
#7675 = AXIS2_PLACEMENT_3D ( 'NONE', #330, #10554, #392 ) ;
#7676 = CARTESIAN_POINT ( 'NONE',  ( -61.99999999999998579, 8.265624999658601979, 2.498450539062049724 ) ) ;
#7677 = FACE_OUTER_BOUND ( 'NONE', #10888, .T. ) ;
#7678 = CARTESIAN_POINT ( 'NONE',  ( -61.99999999999998579, 16.00000000000000000, 1.500000000000002220 ) ) ;
#7679 = CARTESIAN_POINT ( 'NONE',  ( -62.86468353124999453, 9.515624999658600203, 1.500000000000002220 ) ) ;
#7680 = CARTESIAN_POINT ( 'NONE',  ( -62.26794919243111082, 14.04241454900183328, 0.5000000000000013323 ) ) ;
#7681 = VERTEX_POINT ( 'NONE', #10552 ) ;
#7682 = FACE_OUTER_BOUND ( 'NONE', #1436, .T. ) ;
#7683 = CARTESIAN_POINT ( 'NONE',  ( -61.49999999999998579, 12.92708333265053611, 2.366025403784441927 ) ) ;
#7684 = CARTESIAN_POINT ( 'NONE',  ( -61.99999999999999289, 16.01562499965860198, 2.498450539062049724 ) ) ;
#7685 = CARTESIAN_POINT ( 'NONE',  ( -61.13531646874998415, 10.57812499965860198, 1.500000000000002220 ) ) ;
#7686 = CARTESIAN_POINT ( 'NONE',  ( -61.13531646874998415, 15.64062499965860198, 1.500000000000002220 ) ) ;
#7687 = CARTESIAN_POINT ( 'NONE',  ( -61.99999999999998579, 13.03124999931720218, 0.5000000000000013323 ) ) ;
#7688 =( BOUNDED_CURVE ( )  B_SPLINE_CURVE ( 2, ( #7835, #4368, #3659, #3605, #1836, #2777, #7895, #5994, #3548 ),
 .UNSPECIFIED., .F., .T. ) 
 B_SPLINE_CURVE_WITH_KNOTS ( ( 3, 2, 2, 2, 3 ),
 ( 0.2265625000000000000, 0.2291666666666666574, 0.2343750000000000000, 0.2395833333333333426, 0.2421875000000000000 ),
 .UNSPECIFIED. ) 
 CURVE ( )  GEOMETRIC_REPRESENTATION_ITEM ( )  RATIONAL_B_SPLINE_CURVE ( ( 0.9330127018922194093, 0.9330127018922194093, 1.000000000000000000, 0.8660254037844387076, 1.000000000000000000, 0.8660254037844387076, 1.000000000000000000, 0.9330127018922194093, 0.9330127018922194093 ) ) 
 REPRESENTATION_ITEM ( '' )  );
#7689 = ORIENTED_EDGE ( 'NONE', *, *, #2021, .F. ) ;
#7690 = CARTESIAN_POINT ( 'NONE',  ( -61.99999999999998579, 15.06250000000000000, 0.3452994616207497591 ) ) ;
#7691 = CARTESIAN_POINT ( 'NONE',  ( -61.99999999999999289, 9.203124999658601979, 0.5015494609379544944 ) ) ;
#7692 = AXIS2_PLACEMENT_3D ( 'NONE', #2201, #423, #1312 ) ;
#7693 = CARTESIAN_POINT ( 'NONE',  ( -62.49999999999998579, 13.63541666598387003, 2.366025403784441483 ) ) ;
#7694 = CARTESIAN_POINT ( 'NONE',  ( -62.49999999999998579, 13.08333333333333215, 0.6339745962155627357 ) ) ;
#7695 = ORIENTED_EDGE ( 'NONE', *, *, #1166, .T. ) ;
#7696 = EDGE_CURVE ( 'NONE', #4700, #827, #8216, .T. ) ;
#7697 = CARTESIAN_POINT ( 'NONE',  ( -60.99999999999998579, 9.750000000000000000, 1.500000000000002220 ) ) ;
#7698 = CARTESIAN_POINT ( 'NONE',  ( -62.43234176562499016, 11.24479166632526805, 2.248837904296538071 ) ) ;
#7699 = EDGE_CURVE ( 'NONE', #767, #6540, #5487, .T. ) ;
#7700 = CARTESIAN_POINT ( 'NONE',  ( -77.99999999999998579, 0.000000000000000000, 5.000000000000000000 ) ) ;
#7701 = VERTEX_POINT ( 'NONE', #6103 ) ;
#7702 = CARTESIAN_POINT ( 'NONE',  ( -61.99999999999998579, 12.93750000000000000, 2.500000000000002665 ) ) ;
#7703 = CARTESIAN_POINT ( 'NONE',  ( -61.56765823437498142, 12.93229166632526805, 0.7511620957034663704 ) ) ;
#7704 =( NAMED_UNIT ( * ) PLANE_ANGLE_UNIT ( ) SI_UNIT ( $, .RADIAN. ) );
#7705 = DIRECTION ( 'NONE',  ( -0.000000000000000000, -0.000000000000000000, -1.000000000000000000 ) ) ;
#7706 = CARTESIAN_POINT ( 'NONE',  ( -61.49999999999998579, 9.927083332650536107, 2.366025403784441927 ) ) ;
#7707 = ORIENTED_EDGE ( 'NONE', *, *, #7372, .F. ) ;
#7708 = DIRECTION ( 'NONE',  ( -0.000000000000000000, 1.000000000000000000, 0.000000000000000000 ) ) ;
#7709 = ORIENTED_EDGE ( 'NONE', *, *, #7864, .F. ) ;
#7710 = CARTESIAN_POINT ( 'NONE',  ( -61.49999999999998579, 14.79166666666666607, 0.6339745962155628467 ) ) ;
#7711 = CARTESIAN_POINT ( 'NONE',  ( -61.13531646874998415, 11.82812499965860198, 1.500000000000002220 ) ) ;
#7712 = SHAPE_REPRESENTATION_RELATIONSHIP ( 'NONE' , 'NONE' ,  #5016, #6551 ) ;
#7713 = ORIENTED_EDGE ( 'NONE', *, *, #6942, .F. ) ;
#7714 = CARTESIAN_POINT ( 'NONE',  ( -62.86468353124998742, 8.786458332991934128, 1.999225269531025972 ) ) ;
#7715 = CARTESIAN_POINT ( 'NONE',  ( -61.49999999999998579, 14.29166666666666785, 0.6339745962155628467 ) ) ;
#7716 =( BOUNDED_CURVE ( )  B_SPLINE_CURVE ( 2, ( #4496, #3841, #6233, #226, #3787, #400, #2903, #8075, #2010 ),
 .UNSPECIFIED., .F., .F. ) 
 B_SPLINE_CURVE_WITH_KNOTS ( ( 3, 2, 2, 2, 3 ),
 ( 0.3828124999999999445, 0.3854166666666666852, 0.3906250000000000000, 0.3958333333333333148, 0.3984375000000000000 ),
 .UNSPECIFIED. ) 
 CURVE ( )  GEOMETRIC_REPRESENTATION_ITEM ( )  RATIONAL_B_SPLINE_CURVE ( ( 0.9330127018922192983, 0.9330127018922178550, 1.000000000000000000, 0.8660254037844387076, 1.000000000000000000, 0.8660254037844387076, 1.000000000000000000, 0.9330127018922194093, 0.9330127018922194093 ) ) 
 REPRESENTATION_ITEM ( '' )  );
#7717 = EDGE_CURVE ( 'NONE', #2979, #5370, #2892, .T. ) ;
#7718 = CARTESIAN_POINT ( 'NONE',  ( -61.13531646874998415, 13.14062499965860198, 1.500000000000002220 ) ) ;
#7719 = LINE ( 'NONE', #10255, #3774 ) ;
#7720 = VERTEX_POINT ( 'NONE', #1940 ) ;
#7721 = DIRECTION ( 'NONE',  ( -0.000000000000000000, -1.000000000000000000, -0.000000000000000000 ) ) ;
#7722 = EDGE_CURVE ( 'NONE', #9700, #2237, #3264, .T. ) ;
#7723 = VERTEX_POINT ( 'NONE', #1998 ) ;
#7724 = CARTESIAN_POINT ( 'NONE',  ( -61.99999999999998579, 11.53124999931720218, 0.5000000000000013323 ) ) ;
#7725 = CARTESIAN_POINT ( 'NONE',  ( -61.99999999999998579, 14.89062499965860020, 0.5015494609379544944 ) ) ;
#7726 = CARTESIAN_POINT ( 'NONE',  ( -62.26794919243111082, 8.895085449632571084, 2.500000000000003109 ) ) ;
#7727 = DIRECTION ( 'NONE',  ( -1.000000000000000000, 0.000000000000000000, 0.000000000000000000 ) ) ;
#7728 = PLANE ( 'NONE',  #4205 ) ;
#7729 = CARTESIAN_POINT ( 'NONE',  ( -62.86468353124998032, 14.24479166632526983, 1.000774730468978024 ) ) ;
#7730 = CARTESIAN_POINT ( 'NONE',  ( -62.86468353124998032, 8.432291666325266277, 1.000774730468978246 ) ) ;
#7731 = DIRECTION ( 'NONE',  ( -0.000000000000000000, -1.000000000000000000, -0.000000000000000000 ) ) ;
#7732 = DIRECTION ( 'NONE',  ( -0.000000000000000000, -0.000000000000000000, 1.000000000000000000 ) ) ;
#7733 = CARTESIAN_POINT ( 'NONE',  ( -61.99999999999998579, 8.578124999658601979, 2.498450539062049724 ) ) ;
#7734 = CARTESIAN_POINT ( 'NONE',  ( -61.99999999999998579, 10.06250000000000000, 0.5000000000000013323 ) ) ;
#7735 = ORIENTED_EDGE ( 'NONE', *, *, #2693, .F. ) ;
#7736 = CARTESIAN_POINT ( 'NONE',  ( -57.99999999999998579, -10.00000000000000888, 3.000000000000000000 ) ) ;
#7737 = DIRECTION ( 'NONE',  ( 0.000000000000000000, 0.000000000000000000, 1.000000000000000000 ) ) ;
#7738 = CARTESIAN_POINT ( 'NONE',  ( -61.13531646874997705, 15.84895833299193590, 1.000774730468978468 ) ) ;
#7739 = EDGE_CURVE ( 'NONE', #4700, #8255, #10430, .T. ) ;
#7740 = CARTESIAN_POINT ( 'NONE',  ( -61.13531646874998415, 10.82812499965860020, 1.500000000000002220 ) ) ;
#7741 = ADVANCED_BREP_SHAPE_REPRESENTATION ( '', ( #8606, #2307 ), #6386 ) ;
#7742 = CARTESIAN_POINT ( 'NONE',  ( -61.56765823437498142, 8.619791666325268054, 0.7511620957034663704 ) ) ;
#7743 =( NAMED_UNIT ( * ) PLANE_ANGLE_UNIT ( ) SI_UNIT ( $, .RADIAN. ) );
#7744 = ORIENTED_EDGE ( 'NONE', *, *, #851, .T. ) ;
#7745 = CARTESIAN_POINT ( 'NONE',  ( -60.99999999999998579, 15.75000000000000000, 1.500000000000002220 ) ) ;
#7746 = CARTESIAN_POINT ( 'NONE',  ( -62.86468353124998032, 9.494791666325268054, 1.000774730468978024 ) ) ;
#7747 = CARTESIAN_POINT ( 'NONE',  ( -62.99999999999998579, 13.36458333265053433, 2.077350269189627952 ) ) ;
#7748 = CARTESIAN_POINT ( 'NONE',  ( -105.0000000000000000, 2.500000000000000000, 2.000000000000000000 ) ) ;
#7749 = VERTEX_POINT ( 'NONE', #4540 ) ;
#7750 = CARTESIAN_POINT ( 'NONE',  ( -62.49999999999998579, 11.66666666666666785, 2.366025403784441483 ) ) ;
#7751 = CARTESIAN_POINT ( 'NONE',  ( -61.99999999999999289, 11.26562499965860020, 2.498450539062049724 ) ) ;
#7752 = DIRECTION ( 'NONE',  ( 1.000000000000000000, 0.000000000000000000, 0.000000000000000000 ) ) ;
#7753 = EDGE_CURVE ( 'NONE', #8685, #2572, #7456, .T. ) ;
#7754 = DIRECTION ( 'NONE',  ( 1.000000000000000000, 0.000000000000000000, 0.000000000000000000 ) ) ;
#7755 = VERTEX_POINT ( 'NONE', #2274 ) ;
#7756 = CARTESIAN_POINT ( 'NONE',  ( -62.26794919243111082, 12.82366454968462932, 0.5000000000000013323 ) ) ;
#7757 = CARTESIAN_POINT ( 'NONE',  ( -62.86468353124998032, 12.74479166632526805, 1.000774730468978246 ) ) ;
#7758 = CARTESIAN_POINT ( 'NONE',  ( -61.99999999999998579, 10.93750000000000000, 2.500000000000002665 ) ) ;
#7759 = CARTESIAN_POINT ( 'NONE',  ( -62.99999999999998579, 9.093749999317203958, 1.500000000000001998 ) ) ;
#7760 = ORIENTED_EDGE ( 'NONE', *, *, #7387, .F. ) ;
#7761 = EDGE_CURVE ( 'NONE', #6183, #2429, #6559, .T. ) ;
#7762 = ADVANCED_FACE ( 'NONE', ( #656 ), #4922, .T. ) ;
#7763 = VECTOR ( 'NONE', #2046, 1000.000000000000000 ) ;
#7764 = CARTESIAN_POINT ( 'NONE',  ( -61.99999999999998579, 15.28124999931720218, 0.5000000000000013323 ) ) ;
#7765 = CARTESIAN_POINT ( 'NONE',  ( -61.56765823437498852, 11.28645833299193590, 2.248837904296538515 ) ) ;
#7766 =( LENGTH_UNIT ( ) NAMED_UNIT ( * ) SI_UNIT ( .MILLI., .METRE. ) );
#7767 = ORIENTED_EDGE ( 'NONE', *, *, #8905, .F. ) ;
#7768 = VECTOR ( 'NONE', #9554, 1000.000000000000000 ) ;
#7769 = CARTESIAN_POINT ( 'NONE',  ( -61.56765823437498852, 8.848958332991934128, 2.248837904296538515 ) ) ;
#7770 = DIRECTION ( 'NONE',  ( -1.000000000000000000, -0.000000000000000000, -0.000000000000000000 ) ) ;
#7771 = CARTESIAN_POINT ( 'NONE',  ( -61.56765823437498142, 13.93229166632526805, 0.7511620957034663704 ) ) ;
#7772 = CARTESIAN_POINT ( 'NONE',  ( -62.99999999999998579, 9.364583332650536107, 2.077350269189627952 ) ) ;
#7773 = ORIENTED_EDGE ( 'NONE', *, *, #146, .F. ) ;
#7774 = DIRECTION ( 'NONE',  ( -1.000000000000000000, -3.469446951953572774E-16, 0.000000000000000000 ) ) ;
#7775 = CIRCLE ( 'NONE', #9919, 2.500000000000002220 ) ;
#7776 = VECTOR ( 'NONE', #4665, 1000.000000000000000 ) ;
#7777 = ORIENTED_EDGE ( 'NONE', *, *, #320, .F. ) ;
#7778 = CARTESIAN_POINT ( 'NONE',  ( -61.99999999999998579, 10.81250000000000000, 0.5000000000000013323 ) ) ;
#7779 = CARTESIAN_POINT ( 'NONE',  ( -62.49999999999998579, 8.666666666666666075, 2.366025403784441483 ) ) ;
#7780 = DIRECTION ( 'NONE',  ( 0.000000000000000000, 0.000000000000000000, -1.000000000000000000 ) ) ;
#7781 = CYLINDRICAL_SURFACE ( 'NONE', #2283, 1.000000000000000888 ) ;
#7782 =( BOUNDED_CURVE ( )  B_SPLINE_CURVE ( 2, ( #9000, #3267, #660, #507, #7444, #3942, #1443, #8230, #5659 ),
 .UNSPECIFIED., .F., .T. ) 
 B_SPLINE_CURVE_WITH_KNOTS ( ( 3, 2, 2, 2, 3 ),
 ( 0.05468749999999996531, 0.05729166666666666435, 0.06250000000000000000, 0.06770833333333332871, 0.07031250000000001388 ),
 .UNSPECIFIED. ) 
 CURVE ( )  GEOMETRIC_REPRESENTATION_ITEM ( )  RATIONAL_B_SPLINE_CURVE ( ( 0.9330127018922194093, 0.9330127018922185211, 1.000000000000000000, 0.8660254037844387076, 1.000000000000000000, 0.8660254037844387076, 1.000000000000000000, 0.9330127018922189652, 0.9330127018922192983 ) ) 
 REPRESENTATION_ITEM ( '' )  );
#7783 = DIRECTION ( 'NONE',  ( -1.000000000000000000, 0.000000000000000000, 0.000000000000000000 ) ) ;
#7784 = CARTESIAN_POINT ( 'NONE',  ( -61.99999999999999289, 13.57812499965860198, 2.498450539062049724 ) ) ;
#7785 = CARTESIAN_POINT ( 'NONE',  ( -62.86468353124998032, 9.432291666325268054, 1.000774730468978246 ) ) ;
#7786 = EDGE_CURVE ( 'NONE', #7921, #3086, #7386, .T. ) ;
#7787 = CARTESIAN_POINT ( 'NONE',  ( -61.49999999999998579, 9.291666666666666075, 0.6339745962155628467 ) ) ;
#7788 = FACE_OUTER_BOUND ( 'NONE', #1529, .T. ) ;
#7789 = CARTESIAN_POINT ( 'NONE',  ( -61.56765823437498142, 9.682291666325268054, 0.7511620957034663704 ) ) ;
#7790 = AXIS2_PLACEMENT_3D ( 'NONE', #1841, #1894, #2730 ) ;
#7791 = CARTESIAN_POINT ( 'NONE',  ( -61.99999999999998579, 14.15624999931720218, 2.500000000000002665 ) ) ;
#7792 = ORIENTED_EDGE ( 'NONE', *, *, #9135, .T. ) ;
#7793 = DIRECTION ( 'NONE',  ( 0.000000000000000000, 0.000000000000000000, -1.000000000000000000 ) ) ;
#7794 = CARTESIAN_POINT ( 'NONE',  ( -61.99999999999997868, 11.28124999931720041, 0.5000000000000013323 ) ) ;
#7795 = CARTESIAN_POINT ( 'NONE',  ( -61.13531646874997705, 15.05729166632526805, 1.999225269531026417 ) ) ;
#7796 = CARTESIAN_POINT ( 'NONE',  ( -62.43234176562499016, 11.24479166632526805, 2.248837904296538071 ) ) ;
#7797 = CARTESIAN_POINT ( 'NONE',  ( -61.56765823437498852, 8.536458332991934128, 2.248837904296538515 ) ) ;
#7798 = STYLED_ITEM ( 'NONE', ( #1428 ), #7741 ) ;
#7799 = LINE ( 'NONE', #2571, #4454 ) ;
#7800 = ORIENTED_EDGE ( 'NONE', *, *, #8536, .T. ) ;
#7801 = CARTESIAN_POINT ( 'NONE',  ( -61.99999999999998579, 15.31250000000000000, 0.3452994616207497591 ) ) ;
#7802 = CARTESIAN_POINT ( 'NONE',  ( -61.99999999999999289, 9.578124999658600203, 2.498450539062049724 ) ) ;
#7803 = VECTOR ( 'NONE', #3474, 1000.000000000000000 ) ;
#7804 = CARTESIAN_POINT ( 'NONE',  ( -62.99999999999998579, 13.57291666598387359, 0.9226497308103756012 ) ) ;
#7805 = CARTESIAN_POINT ( 'NONE',  ( -61.99999999999998579, 8.906249999317202182, 2.500000000000002665 ) ) ;
#7806 = ORIENTED_EDGE ( 'NONE', *, *, #5198, .F. ) ;
#7807 = ADVANCED_FACE ( 'NONE', ( #10822 ), #7628, .T. ) ;
#7808 = DIRECTION ( 'NONE',  ( -1.000000000000000000, -0.000000000000000000, -0.000000000000000000 ) ) ;
#7809 = AXIS2_PLACEMENT_3D ( 'NONE', #5280, #8689, #4335 ) ;
#7810 = CARTESIAN_POINT ( 'NONE',  ( -61.13531646874997705, 12.09895833299193235, 1.000774730468978468 ) ) ;
#7811 = VECTOR ( 'NONE', #10317, 1000.000000000000000 ) ;
#7812 = CARTESIAN_POINT ( 'NONE',  ( -105.0000000000000000, -2.500000000000000000, 3.000000000000000000 ) ) ;
#7813 = ORIENTED_EDGE ( 'NONE', *, *, #4377, .T. ) ;
#7814 = CARTESIAN_POINT ( 'NONE',  ( -61.99999999999998579, 10.93750000000000000, 2.654700538379254571 ) ) ;
#7815 = CARTESIAN_POINT ( 'NONE',  ( -62.99999999999998579, 10.10416666666666785, 0.9226497308103756012 ) ) ;
#7816 = CARTESIAN_POINT ( 'NONE',  ( -61.13531646874998415, 13.89062499965860198, 1.500000000000002220 ) ) ;
#7817 = DIRECTION ( 'NONE',  ( 0.000000000000000000, 0.000000000000000000, -1.000000000000000000 ) ) ;
#7818 = CARTESIAN_POINT ( 'NONE',  ( -62.99999999999998579, 9.114583332650537884, 2.077350269189627952 ) ) ;
#7819 = ORIENTED_EDGE ( 'NONE', *, *, #7525, .F. ) ;
#7820 = DIRECTION ( 'NONE',  ( -0.000000000000000000, -0.000000000000000000, -1.000000000000000000 ) ) ;
#7821 = CARTESIAN_POINT ( 'NONE',  ( -37.99999999999999289, -14.00000000000000888, 3.000000000000000000 ) ) ;
#7822 = CARTESIAN_POINT ( 'NONE',  ( -61.99999999999998579, 11.01562499965859843, 2.498450539062049724 ) ) ;
#7823 = ORIENTED_EDGE ( 'NONE', *, *, #1694, .F. ) ;
#7824 = CARTESIAN_POINT ( 'NONE',  ( -61.13531646874998415, 10.66145833299193413, 1.000774730468978468 ) ) ;
#7825 = CARTESIAN_POINT ( 'NONE',  ( -62.99999999999998579, 15.59374999931720218, 1.500000000000001998 ) ) ;
#7826 = CARTESIAN_POINT ( 'NONE',  ( -61.99999999999998579, 14.70312499965860020, 0.5015494609379544944 ) ) ;
#7827 = CARTESIAN_POINT ( 'NONE',  ( -61.49999999999998579, 8.260416665983870033, 0.6339745962155628467 ) ) ;
#7828 = ORIENTED_EDGE ( 'NONE', *, *, #4087, .F. ) ;
#7829 = DIRECTION ( 'NONE',  ( -0.000000000000000000, -1.000000000000000000, -0.000000000000000000 ) ) ;
#7830 = VECTOR ( 'NONE', #9412, 1000.000000000000000 ) ;
#7831 = VERTEX_POINT ( 'NONE', #9885 ) ;
#7832 = CARTESIAN_POINT ( 'NONE',  ( -61.49999999999998579, 12.76041666598386826, 0.6339745962155628467 ) ) ;
#7833 = ADVANCED_FACE ( 'NONE', ( #10766 ), #2325, .T. ) ;
#7834 = CARTESIAN_POINT ( 'NONE',  ( -62.43234176562498305, 15.91145833299193590, 0.7511620957034662593 ) ) ;
#7835 = CARTESIAN_POINT ( 'NONE',  ( -61.99999999999998579, 9.812500000000000000, 0.5000000000000013323 ) ) ;
#7836 = FACE_OUTER_BOUND ( 'NONE', #7381, .T. ) ;
#7837 = CARTESIAN_POINT ( 'NONE',  ( -46.99999999999998579, -18.00000000000001066, 3.000000000000000000 ) ) ;
#7838 = CARTESIAN_POINT ( 'NONE',  ( -62.43234176562498305, 14.47395833299193413, 0.7511620957034662593 ) ) ;
#7839 = CARTESIAN_POINT ( 'NONE',  ( -62.43234176562499016, 9.244791666325268054, 2.248837904296538071 ) ) ;
#7840 = CARTESIAN_POINT ( 'NONE',  ( -61.99999999999998579, 16.00000000000000000, 1.500000000000002220 ) ) ;
#7841 = CARTESIAN_POINT ( 'NONE',  ( -62.99999999999998579, 9.625000000000000000, 1.500000000000001998 ) ) ;
#7842 = CLOSED_SHELL ( 'NONE', ( #6823, #8569, #2271, #6724, #1106, #6743, #2769, #7807, #6029, #6448, #9197, #3874, #9022 ) ) ;
#7843 = CARTESIAN_POINT ( 'NONE',  ( -61.13531646874998415, 10.61979166632526983, 1.999225269531026417 ) ) ;
#7844 = FACE_OUTER_BOUND ( 'NONE', #9018, .T. ) ;
#7845 = ORIENTED_EDGE ( 'NONE', *, *, #8698, .T. ) ;
#7846 = CARTESIAN_POINT ( 'NONE',  ( 0.2309054577385449836, -0.2499999999999997780, -1.812959136724909603 ) ) ;
#7847 = CARTESIAN_POINT ( 'NONE',  ( -61.49999999999998579, 13.01041666598386826, 0.6339745962155628467 ) ) ;
#7848 =( BOUNDED_CURVE ( )  B_SPLINE_CURVE ( 2, ( #7687, #2740, #4227, #5221, #10175, #5957, #8574, #10222, #2624 ),
 .UNSPECIFIED., .F., .T. ) 
 B_SPLINE_CURVE_WITH_KNOTS ( ( 3, 2, 2, 2, 3 ),
 ( 0.6015625000000000000, 0.6041666666666666297, 0.6093750000000000000, 0.6145833333333333703, 0.6171875000000000000 ),
 .UNSPECIFIED. ) 
 CURVE ( )  GEOMETRIC_REPRESENTATION_ITEM ( )  RATIONAL_B_SPLINE_CURVE ( ( 0.9330127018922194093, 0.9330127018922194093, 1.000000000000000000, 0.8660254037844387076, 1.000000000000000000, 0.8660254037844387076, 1.000000000000000000, 0.9330127018922194093, 0.9330127018922194093 ) ) 
 REPRESENTATION_ITEM ( '' )  );
#7849 = VECTOR ( 'NONE', #1771, 1000.000000000000000 ) ;
#7850 = CARTESIAN_POINT ( 'NONE',  ( -62.86468353124998032, 15.18229166632526805, 1.000774730468978024 ) ) ;
#7851 = CARTESIAN_POINT ( 'NONE',  ( -62.43234176562498305, 12.66145833299193413, 0.7511620957034662593 ) ) ;
#7852 = AXIS2_PLACEMENT_3D ( 'NONE', #465, #5328, #10568 ) ;
#7853 = CARTESIAN_POINT ( 'NONE',  ( -61.99999999999999289, 8.515624999658601979, 2.498450539062049724 ) ) ;
#7854 = DIRECTION ( 'NONE',  ( -1.000000000000000000, 0.000000000000000000, 0.000000000000000000 ) ) ;
#7855 = EDGE_LOOP ( 'NONE', ( #489, #726, #8999, #205 ) ) ;
#7856 = CARTESIAN_POINT ( 'NONE',  ( -61.73205080756884655, 8.520085449632571084, 0.4999999999999994449 ) ) ;
#7857 = CARTESIAN_POINT ( 'NONE',  ( -61.13531646874997705, 9.411458332991935904, 1.000774730468978468 ) ) ;
#7858 =( NAMED_UNIT ( * ) PLANE_ANGLE_UNIT ( ) SI_UNIT ( $, .RADIAN. ) );
#7859 = CARTESIAN_POINT ( 'NONE',  ( -61.13531646874998415, 15.84895833299193413, 1.000774730468978468 ) ) ;
#7860 = CARTESIAN_POINT ( 'NONE',  ( -62.49999999999998579, 15.05208333265053611, 0.6339745962155627357 ) ) ;
#7861 = DIRECTION ( 'NONE',  ( 0.000000000000000000, 0.000000000000000000, -1.000000000000000000 ) ) ;
#7862 = ORIENTED_EDGE ( 'NONE', *, *, #602, .F. ) ;
#7863 = VECTOR ( 'NONE', #7627, 1000.000000000000000 ) ;
#7864 = EDGE_CURVE ( 'NONE', #9204, #3994, #10664, .T. ) ;
#7865 = AXIS2_PLACEMENT_3D ( 'NONE', #3141, #10803, #1577 ) ;
#7866 = DIRECTION ( 'NONE',  ( -0.000000000000000000, -0.000000000000000000, 1.000000000000000000 ) ) ;
#7867 = EDGE_CURVE ( 'NONE', #2572, #570, #3157, .T. ) ;
#7868 = CARTESIAN_POINT ( 'NONE',  ( -62.43234176562499016, 11.99479166632526628, 2.248837904296538071 ) ) ;
#7869 = CARTESIAN_POINT ( 'NONE',  ( -61.99999999999998579, 8.265624999658601979, 2.498450539062049724 ) ) ;
#7870 = CARTESIAN_POINT ( 'NONE',  ( -53.99999999999999289, 3.061616997868382254E-15, 13.00000000000000178 ) ) ;
#7871 = VERTEX_POINT ( 'NONE', #6454 ) ;
#7872 = CARTESIAN_POINT ( 'NONE',  ( -61.99999999999998579, 10.56250000000000000, 0.3452994616207497591 ) ) ;
#7873 = AXIS2_PLACEMENT_3D ( 'NONE', #4992, #6784, #780 ) ;
#7874 = EDGE_CURVE ( 'NONE', #2754, #9906, #613, .T. ) ;
#7875 = CARTESIAN_POINT ( 'NONE',  ( -62.86468353124998742, 14.03645833299193590, 1.999225269531025972 ) ) ;
#7876 = CARTESIAN_POINT ( 'NONE',  ( -62.49999999999998579, 13.83333333333333215, 0.6339745962155627357 ) ) ;
#7877 = CARTESIAN_POINT ( 'NONE',  ( -60.99999999999998579, 8.968749999317203958, 1.500000000000002220 ) ) ;
#7878 = PRODUCT_RELATED_PRODUCT_CATEGORY ( 'part', '', ( #5186 ) ) ;
#7879 = EDGE_LOOP ( 'NONE', ( #763, #8809, #3416, #10374 ) ) ;
#7880 = DIRECTION ( 'NONE',  ( -1.000000000000000000, -0.000000000000000000, -0.000000000000000000 ) ) ;
#7881 = AXIS2_PLACEMENT_3D ( 'NONE', #2174, #453, #1345 ) ;
#7882 = DIRECTION ( 'NONE',  ( -0.000000000000000000, -0.000000000000000000, -1.000000000000000000 ) ) ;
#7883 = CARTESIAN_POINT ( 'NONE',  ( -62.86468353124999453, 10.70312499965860020, 1.500000000000002220 ) ) ;
#7884 = ORIENTED_EDGE ( 'NONE', *, *, #6829, .F. ) ;
#7885 = EDGE_CURVE ( 'NONE', #1211, #7362, #7440, .T. ) ;
#7886 = ADVANCED_BREP_SHAPE_REPRESENTATION ( '', ( #8465, #2307 ), #6012 ) ;
#7887 = CARTESIAN_POINT ( 'NONE',  ( -61.13531646874998415, 9.869791666325269830, 1.999225269531026417 ) ) ;
#7888 = CARTESIAN_POINT ( 'NONE',  ( -61.99999999999998579, 15.90624999931719863, 2.500000000000002665 ) ) ;
#7889 = CARTESIAN_POINT ( 'NONE',  ( -61.99999999999998579, 14.82812499965860020, 2.498450539062049724 ) ) ;
#7890 = DIRECTION ( 'NONE',  ( -0.000000000000000000, -0.000000000000000000, 1.000000000000000000 ) ) ;
#7891 = ORIENTED_EDGE ( 'NONE', *, *, #10878, .T. ) ;
#7892 = CARTESIAN_POINT ( 'NONE',  ( 8.300922883092140858E-17, -0.2499999999999997780, -1.455170506525537588 ) ) ;
#7893 = ORIENTED_EDGE ( 'NONE', *, *, #646, .F. ) ;
#7894 = CARTESIAN_POINT ( 'NONE',  ( -60.99999999999998579, 8.729166666666666075, 2.077350269189628840 ) ) ;
#7895 = CARTESIAN_POINT ( 'NONE',  ( -62.49999999999998579, 9.916666666666667851, 2.366025403784441483 ) ) ;
#7896 = LINE ( 'NONE', #2004, #4583 ) ;
#7897 = EDGE_CURVE ( 'NONE', #5429, #1066, #9055, .T. ) ;
#7898 = DIRECTION ( 'NONE',  ( -0.000000000000000000, -0.000000000000000000, 1.000000000000000000 ) ) ;
#7899 = CARTESIAN_POINT ( 'NONE',  ( -61.13531646874998415, 13.64062499965860198, 1.500000000000002220 ) ) ;
#7900 = CARTESIAN_POINT ( 'NONE',  ( -61.56765823437498142, 10.61979166632526805, 0.7511620957034663704 ) ) ;
#7901 = CARTESIAN_POINT ( 'NONE',  ( -61.99999999999998579, 11.56250000000000000, 0.5000000000000013323 ) ) ;
#7902 = LINE ( 'NONE', #7179, #2643 ) ;
#7903 = CARTESIAN_POINT ( 'NONE',  ( -62.86468353124998032, 10.74479166632526628, 1.000774730468978246 ) ) ;
#7904 = ORIENTED_EDGE ( 'NONE', *, *, #3790, .T. ) ;
#7905 = DIRECTION ( 'NONE',  ( 1.000000000000000000, 0.000000000000000000, 0.000000000000000000 ) ) ;
#7906 = ADVANCED_FACE ( 'NONE', ( #8273 ), #2852, .F. ) ;
#7907 = CARTESIAN_POINT ( 'NONE',  ( -61.49999999999998579, 11.17708333265053611, 2.366025403784441927 ) ) ;
#7908 = CARTESIAN_POINT ( 'NONE',  ( -61.73205080756886076, 10.05133545031537068, 0.5000000000000014433 ) ) ;
#7909 = CARTESIAN_POINT ( 'NONE',  ( -61.99999999999998579, 12.51562499965860198, 2.498450539062049724 ) ) ;
#7910 = CARTESIAN_POINT ( 'NONE',  ( -61.13531646874998415, 9.078124999658601979, 1.500000000000002220 ) ) ;
#7911 = DIRECTION ( 'NONE',  ( 1.000000000000000000, 0.000000000000000000, 0.000000000000000000 ) ) ;
#7912 = ORIENTED_EDGE ( 'NONE', *, *, #8187, .T. ) ;
#7913 = CARTESIAN_POINT ( 'NONE',  ( -62.99999999999998579, 10.86458333265053611, 2.077350269189627952 ) ) ;
#7914 = CARTESIAN_POINT ( 'NONE',  ( -62.86468353124999453, 10.01562499965860198, 1.500000000000002220 ) ) ;
#7915 = DIRECTION ( 'NONE',  ( 1.000000000000000000, 0.000000000000000000, 0.000000000000000000 ) ) ;
#7916 = CARTESIAN_POINT ( 'NONE',  ( -61.99999999999998579, 15.51562499965860198, 2.498450539062049724 ) ) ;
#7917 = CARTESIAN_POINT ( 'NONE',  ( -62.99999999999998579, 14.36458333265053611, 2.077350269189627952 ) ) ;
#7918 = CARTESIAN_POINT ( 'NONE',  ( -61.99999999999998579, 14.68750000000000000, 2.500000000000002665 ) ) ;
#7919 = VERTEX_POINT ( 'NONE', #2375 ) ;
#7920 = FACE_OUTER_BOUND ( 'NONE', #8894, .T. ) ;
#7921 = VERTEX_POINT ( 'NONE', #713 ) ;
#7922 =( BOUNDED_CURVE ( )  B_SPLINE_CURVE ( 2, ( #1554, #5616, #7399, #10778, #3170, #9008, #9955, #1402, #4882 ),
 .UNSPECIFIED., .F., .T. ) 
 B_SPLINE_CURVE_WITH_KNOTS ( ( 3, 2, 2, 2, 3 ),
 ( 0.1171875000000000278, 0.1197916666666666713, 0.1250000000000000000, 0.1302083333333333426, 0.1328125000000000000 ),
 .UNSPECIFIED. ) 
 CURVE ( )  GEOMETRIC_REPRESENTATION_ITEM ( )  RATIONAL_B_SPLINE_CURVE ( ( 0.9330127018922194093, 0.9330127018922200755, 1.000000000000000000, 0.8660254037844387076, 1.000000000000000000, 0.8660254037844387076, 1.000000000000000000, 0.9330127018922194093, 0.9330127018922194093 ) ) 
 REPRESENTATION_ITEM ( '' )  );
#7923 = CARTESIAN_POINT ( 'NONE',  ( -61.56765823437498852, 12.53645833299193413, 2.248837904296538515 ) ) ;
#7924 = CARTESIAN_POINT ( 'NONE',  ( -61.13531646874998415, 8.328124999658601979, 1.500000000000002220 ) ) ;
#7925 = DIRECTION ( 'NONE',  ( 0.000000000000000000, 1.000000000000000000, 0.000000000000000000 ) ) ;
#7926 = EDGE_LOOP ( 'NONE', ( #3777, #4207, #7224 ) ) ;
#7927 = CARTESIAN_POINT ( 'NONE',  ( -62.49999999999998579, 11.91666666666666607, 2.366025403784441483 ) ) ;
#7928 = CARTESIAN_POINT ( 'NONE',  ( -62.49999999999998579, 10.08333333333333215, 0.6339745962155627357 ) ) ;
#7929 = CARTESIAN_POINT ( 'NONE',  ( -62.86468353124998742, 14.78645833299193413, 1.999225269531025972 ) ) ;
#7930 =( LENGTH_UNIT ( ) NAMED_UNIT ( * ) SI_UNIT ( .MILLI., .METRE. ) );
#7931 = CARTESIAN_POINT ( 'NONE',  ( -61.99999999999998579, 13.43749999999999822, 2.500000000000002665 ) ) ;
#7932 = CARTESIAN_POINT ( 'NONE',  ( -61.49999999999998579, 10.17708333265053611, 2.366025403784441927 ) ) ;
#7933 = ADVANCED_FACE ( 'NONE', ( #9157 ), #4818, .F. ) ;
#7934 = ORIENTED_EDGE ( 'NONE', *, *, #7187, .F. ) ;
#7935 = CARTESIAN_POINT ( 'NONE',  ( -61.99999999999998579, 11.15624999931720218, 2.500000000000002665 ) ) ;
#7936 = DIRECTION ( 'NONE',  ( 1.000000000000000000, 0.000000000000000000, 0.000000000000000000 ) ) ;
#7937 = CARTESIAN_POINT ( 'NONE',  ( -62.43234176562499016, 11.74479166632526805, 2.248837904296538071 ) ) ;
#7938 = ORIENTED_EDGE ( 'NONE', *, *, #3189, .T. ) ;
#7939 = CARTESIAN_POINT ( 'NONE',  ( -62.43234176562498305, 10.72395833299193413, 0.7511620957034662593 ) ) ;
#7940 = LINE ( 'NONE', #8891, #5464 ) ;
#7941 = CARTESIAN_POINT ( 'NONE',  ( -61.56765823437498852, 13.84895833299193413, 2.248837904296538515 ) ) ;
#7942 = DIRECTION ( 'NONE',  ( 0.000000000000000000, 1.000000000000000000, 0.000000000000000000 ) ) ;
#7943 = EDGE_LOOP ( 'NONE', ( #6888, #8736, #4355, #9225 ) ) ;
#7944 = CARTESIAN_POINT ( 'NONE',  ( -61.73205080756886076, 10.55133545031537068, 0.5000000000000014433 ) ) ;
#7945 = ADVANCED_FACE ( 'NONE', ( #6393 ), #9780, .T. ) ;
#7946 = AXIS2_PLACEMENT_3D ( 'NONE', #10924, #8430, #8378 ) ;
#7947 = ORIENTED_EDGE ( 'NONE', *, *, #1288, .T. ) ;
#7948 = CARTESIAN_POINT ( 'NONE',  ( -62.99999999999998579, 15.09374999931720218, 1.500000000000001998 ) ) ;
#7949 = CARTESIAN_POINT ( 'NONE',  ( -62.99999999999998579, 8.604166666666666075, 0.9226497308103756012 ) ) ;
#7950 = DIRECTION ( 'NONE',  ( 0.000000000000000000, 0.000000000000000000, -1.000000000000000000 ) ) ;
#7951 = CARTESIAN_POINT ( 'NONE',  ( -61.73205080756886076, 16.16741454900183328, 2.500000000000003109 ) ) ;
#7952 = DIRECTION ( 'NONE',  ( -1.000000000000000000, -0.000000000000000000, -0.000000000000000000 ) ) ;
#7953 = CARTESIAN_POINT ( 'NONE',  ( -62.43234176562499016, 13.55729166632526805, 2.248837904296538071 ) ) ;
#7954 = CARTESIAN_POINT ( 'NONE',  ( -61.99999999999998579, 10.26562499965860376, 2.498450539062049724 ) ) ;
#7955 = UNCERTAINTY_MEASURE_WITH_UNIT (LENGTH_MEASURE( 1.000000000000000082E-05 ), #3880, 'distance_accuracy_value', 'NONE');
#7956 = CARTESIAN_POINT ( 'NONE',  ( -61.49999999999998579, 11.92708333265053611, 2.366025403784441927 ) ) ;
#7957 = CARTESIAN_POINT ( 'NONE',  ( 0.000000000000000000, 0.2499999999999998335, 2.000000000000000000 ) ) ;
#7958 = CARTESIAN_POINT ( 'NONE',  ( -61.56765823437498852, 10.09895833299193413, 2.248837904296538515 ) ) ;
#7959 = CARTESIAN_POINT ( 'NONE',  ( -62.26794919243111082, 12.17633545031537068, 2.500000000000003109 ) ) ;
#7960 = ORIENTED_EDGE ( 'NONE', *, *, #7717, .T. ) ;
#7961 = CARTESIAN_POINT ( 'NONE',  ( -60.99999999999998579, 13.98958333265053611, 0.9226497308103762673 ) ) ;
#7962 = LINE ( 'NONE', #9623, #2368 ) ;
#7963 = AXIS2_PLACEMENT_3D ( 'NONE', #6993, #2943, #10371 ) ;
#7964 = ORIENTED_EDGE ( 'NONE', *, *, #91, .T. ) ;
#7965 = CARTESIAN_POINT ( 'NONE',  ( -61.99999999999998579, 10.06250000000000000, 0.5000000000000013323 ) ) ;
#7966 = CARTESIAN_POINT ( 'NONE',  ( -61.13531646874998415, 12.34895833299193413, 1.000774730468978468 ) ) ;
#7967 = VECTOR ( 'NONE', #164, 1000.000000000000000 ) ;
#7968 = CARTESIAN_POINT ( 'NONE',  ( -62.86468353124999453, 9.453124999658600203, 1.500000000000002220 ) ) ;
#7969 = DIRECTION ( 'NONE',  ( 0.000000000000000000, 0.000000000000000000, 1.000000000000000000 ) ) ;
#7970 = ORIENTED_EDGE ( 'NONE', *, *, #4185, .T. ) ;
#7971 = CARTESIAN_POINT ( 'NONE',  ( -62.99999999999998579, 15.89583333333333037, 2.077350269189627952 ) ) ;
#7972 = CARTESIAN_POINT ( 'NONE',  ( -62.43234176562498305, 9.473958332991935904, 0.7511620957034662593 ) ) ;
#7973 = AXIS2_PLACEMENT_3D ( 'NONE', #5036, #2492, #5142 ) ;
#7974 = CARTESIAN_POINT ( 'NONE',  ( -61.99999999999998579, 14.89062499965860020, 0.5015494609379544944 ) ) ;
#7975 = CARTESIAN_POINT ( 'NONE',  ( -61.49999999999998579, 14.51041666598387003, 0.6339745962155628467 ) ) ;
#7976 = FACE_OUTER_BOUND ( 'NONE', #1340, .T. ) ;
#7977 = ORIENTED_EDGE ( 'NONE', *, *, #2887, .T. ) ;
#7978 = CARTESIAN_POINT ( 'NONE',  ( 0.000000000000000000, 0.000000000000000000, 2.000000000000000000 ) ) ;
#7979 = VECTOR ( 'NONE', #5948, 1000.000000000000000 ) ;
#7980 = ORIENTED_EDGE ( 'NONE', *, *, #1631, .T. ) ;
#7981 = CARTESIAN_POINT ( 'NONE',  ( -62.43234176562498305, 12.41145833299193413, 0.7511620957034662593 ) ) ;
#7982 = CARTESIAN_POINT ( 'NONE',  ( -61.56765823437498142, 8.869791666325268054, 0.7511620957034663704 ) ) ;
#7983 = VERTEX_POINT ( 'NONE', #3888 ) ;
#7984 = CARTESIAN_POINT ( 'NONE',  ( -60.99999999999998579, 12.77083333333333393, 0.9226497308103762673 ) ) ;
#7985 = EDGE_CURVE ( 'NONE', #9736, #9380, #9583, .T. ) ;
#7986 = CARTESIAN_POINT ( 'NONE',  ( -105.0000000000000000, 2.500000000000000000, 2.000000000000000000 ) ) ;
#7987 = VECTOR ( 'NONE', #6642, 1000.000000000000000 ) ;
#7988 = CARTESIAN_POINT ( 'NONE',  ( -62.86468353124998742, 14.53645833299193413, 1.999225269531025972 ) ) ;
#7989 = CARTESIAN_POINT ( 'NONE',  ( -62.99999999999998579, 13.89583333333333215, 2.077350269189627952 ) ) ;
#7990 = CARTESIAN_POINT ( 'NONE',  ( -60.99999999999998579, 11.23958333265053788, 0.9226497308103762673 ) ) ;
#7991 = ORIENTED_EDGE ( 'NONE', *, *, #10276, .T. ) ;
#7992 = LINE ( 'NONE', #6534, #6200 ) ;
#7993 = DIRECTION ( 'NONE',  ( 0.000000000000000000, 0.000000000000000000, -1.000000000000000000 ) ) ;
#7994 = AXIS2_PLACEMENT_3D ( 'NONE', #6673, #4936, #2287 ) ;
#7995 = CARTESIAN_POINT ( 'NONE',  ( -62.86468353124998742, 12.22395833299193413, 1.999225269531025972 ) ) ;
#7996 = DIRECTION ( 'NONE',  ( -1.000000000000000000, -0.000000000000000000, -0.000000000000000000 ) ) ;
#7997 = ADVANCED_FACE ( 'NONE', ( #8482 ), #3915, .T. ) ;
#7998 = VERTEX_POINT ( 'NONE', #10978 ) ;
#7999 = CARTESIAN_POINT ( 'NONE',  ( -61.13531646874998415, 9.619791666325268054, 1.999225269531026417 ) ) ;
#8000 = CARTESIAN_POINT ( 'NONE',  ( -49.99999999999998579, -15.00000000000001243, -2.000000000000000000 ) ) ;
#8001 = CARTESIAN_POINT ( 'NONE',  ( -62.86468353124998032, 13.99479166632526983, 1.000774730468978246 ) ) ;
#8002 = DIRECTION ( 'NONE',  ( -1.000000000000000000, 0.000000000000000000, 0.000000000000000000 ) ) ;
#8003 = ORIENTED_EDGE ( 'NONE', *, *, #795, .T. ) ;
#8004 = DIRECTION ( 'NONE',  ( 0.000000000000000000, 1.000000000000000000, 0.000000000000000000 ) ) ;
#8005 = EDGE_CURVE ( 'NONE', #918, #8888, #1810, .T. ) ;
#8006 = ORIENTED_EDGE ( 'NONE', *, *, #2401, .T. ) ;
#8007 = PLANE ( 'NONE',  #9442 ) ;
#8008 = CARTESIAN_POINT ( 'NONE',  ( -62.49999999999998579, 8.333333333333333925, 0.6339745962155627357 ) ) ;
#8009 = CARTESIAN_POINT ( 'NONE',  ( -61.99999999999998579, 16.00000000000000000, 2.500000000000000444 ) ) ;
#8010 = LINE ( 'NONE', #3660, #4932 ) ;
#8011 = DIRECTION ( 'NONE',  ( 0.000000000000000000, 0.000000000000000000, 1.000000000000000000 ) ) ;
#8012 = CARTESIAN_POINT ( 'NONE',  ( -62.43234176562498305, 14.97395833299193590, 0.7511620957034662593 ) ) ;
#8013 = ADVANCED_FACE ( 'NONE', ( #5135 ), #6765, .T. ) ;
#8014 = CARTESIAN_POINT ( 'NONE',  ( -62.86468353124998742, 9.973958332991932352, 1.999225269531025972 ) ) ;
#8015 = CARTESIAN_POINT ( 'NONE',  ( -62.49999999999998579, 9.583333333333332149, 0.6339745962155627357 ) ) ;
#8016 = CARTESIAN_POINT ( 'NONE',  ( -61.56765823437498852, 11.09895833299193590, 2.248837904296538515 ) ) ;
#8017 = FACE_OUTER_BOUND ( 'NONE', #1661, .T. ) ;
#8018 = ORIENTED_EDGE ( 'NONE', *, *, #555, .T. ) ;
#8019 = CARTESIAN_POINT ( 'NONE',  ( -62.26794919243111082, 14.42633545031536890, 2.500000000000003109 ) ) ;
#8020 = DIRECTION ( 'NONE',  ( -1.000000000000000000, 0.000000000000000000, 0.000000000000000000 ) ) ;
#8021 = VERTEX_POINT ( 'NONE', #9366 ) ;
#8022 = CARTESIAN_POINT ( 'NONE',  ( -62.26794919243111082, 10.39508544963257286, 2.500000000000003109 ) ) ;
#8023 = CARTESIAN_POINT ( 'NONE',  ( -62.86468353124998032, 13.18229166632526805, 1.000774730468978246 ) ) ;
#8024 = CARTESIAN_POINT ( 'NONE',  ( -62.86468353124998032, 10.68229166632526628, 1.000774730468978024 ) ) ;
#8025 = DIRECTION ( 'NONE',  ( -0.000000000000000000, -1.000000000000000000, -0.000000000000000000 ) ) ;
#8026 = VERTEX_POINT ( 'NONE', #90 ) ;
#8027 = CARTESIAN_POINT ( 'NONE',  ( -61.49999999999998579, 15.79166666666666607, 0.6339745962155628467 ) ) ;
#8028 = AXIS2_PLACEMENT_3D ( 'NONE', #10215, #3556, #8508 ) ;
#8029 = CARTESIAN_POINT ( 'NONE',  ( -62.43234176562498305, 11.72395833299193590, 0.7511620957034662593 ) ) ;
#8030 = APPLICATION_PROTOCOL_DEFINITION ( 'draft international standard', 'automotive_design', 1998, #4975 ) ;
#8031 = CARTESIAN_POINT ( 'NONE',  ( -61.56765823437498852, 15.28645833299193590, 2.248837904296538515 ) ) ;
#8032 = CARTESIAN_POINT ( 'NONE',  ( -61.99999999999998579, 15.03124999931720041, 0.3452994616207497591 ) ) ;
#8033 = CARTESIAN_POINT ( 'NONE',  ( -62.49999999999998579, 16.05208333265053255, 0.6339745962155627357 ) ) ;
#8034 = VERTEX_POINT ( 'NONE', #5870 ) ;
#8035 = CARTESIAN_POINT ( 'NONE',  ( -61.49999999999998579, 16.01041666598386826, 0.6339745962155628467 ) ) ;
#8036 = ORIENTED_EDGE ( 'NONE', *, *, #5916, .T. ) ;
#8037 = AXIS2_PLACEMENT_3D ( 'NONE', #774, #10733, #9167 ) ;
#8038 = EDGE_CURVE ( 'NONE', #7493, #1608, #5136, .T. ) ;
#8039 = CARTESIAN_POINT ( 'NONE',  ( -61.99999999999999289, 13.26562499965859843, 2.498450539062049724 ) ) ;
#8040 = CARTESIAN_POINT ( 'NONE',  ( -61.99999999999998579, 8.515624999658601979, 2.498450539062049724 ) ) ;
#8041 = DIRECTION ( 'NONE',  ( -0.000000000000000000, -0.000000000000000000, -1.000000000000000000 ) ) ;
#8042 = ORIENTED_EDGE ( 'NONE', *, *, #1779, .F. ) ;
#8043 = CARTESIAN_POINT ( 'NONE',  ( -60.99999999999998579, 11.77083333333333393, 0.9226497308103762673 ) ) ;
#8044 = LINE ( 'NONE', #10534, #9099 ) ;
#8045 = CARTESIAN_POINT ( 'NONE',  ( -62.43234176562499016, 14.55729166632526983, 2.248837904296538071 ) ) ;
#8046 = ADVANCED_FACE ( 'NONE', ( #6037 ), #9421, .T. ) ;
#8047 = CARTESIAN_POINT ( 'NONE',  ( -62.99999999999998579, 14.34374999931720041, 1.500000000000001998 ) ) ;
#8048 = AXIS2_PLACEMENT_3D ( 'NONE', #5005, #5690, #12 ) ;
#8049 = AXIS2_PLACEMENT_3D ( 'NONE', #2038, #7094, #372 ) ;
#8050 = CARTESIAN_POINT ( 'NONE',  ( -62.49999999999998579, 11.05208333265053611, 0.6339745962155627357 ) ) ;
#8051 = ORIENTED_EDGE ( 'NONE', *, *, #8420, .T. ) ;
#8052 = CARTESIAN_POINT ( 'NONE',  ( -61.99999999999998579, 16.00000000000000000, 1.500000000000002220 ) ) ;
#8053 = EDGE_CURVE ( 'NONE', #2251, #2222, #5080, .T. ) ;
#8054 = CIRCLE ( 'NONE', #4301, 1.000000000000000888 ) ;
#8055 = CARTESIAN_POINT ( 'NONE',  ( -61.99999999999998579, 12.64062499965860198, 0.5015494609379544944 ) ) ;
#8056 = SURFACE_SIDE_STYLE ('',( #494 ) ) ;
#8057 = ORIENTED_EDGE ( 'NONE', *, *, #8550, .T. ) ;
#8058 = CARTESIAN_POINT ( 'NONE',  ( -62.43234176562499016, 10.55729166632526983, 2.248837904296538071 ) ) ;
#8059 =( BOUNDED_CURVE ( )  B_SPLINE_CURVE ( 2, ( #253, #2211, #10755, #10806, #3872, #2986, #9926, #6372, #3144 ),
 .UNSPECIFIED., .F., .T. ) 
 B_SPLINE_CURVE_WITH_KNOTS ( ( 3, 2, 2, 2, 3 ),
 ( 0.03906250000000003469, 0.04166666666666666435, 0.04687500000000000000, 0.05208333333333333565, 0.05468749999999996531 ),
 .UNSPECIFIED. ) 
 CURVE ( )  GEOMETRIC_REPRESENTATION_ITEM ( )  RATIONAL_B_SPLINE_CURVE ( ( 0.9330127018922194093, 0.9330127018922202975, 1.000000000000000000, 0.8660254037844387076, 1.000000000000000000, 0.8660254037844387076, 1.000000000000000000, 0.9330127018922202975, 0.9330127018922194093 ) ) 
 REPRESENTATION_ITEM ( '' )  );
#8060 = CARTESIAN_POINT ( 'NONE',  ( 0.000000000000000000, -0.2499999999999997224, -2.000000000000000000 ) ) ;
#8061 = AXIS2_PLACEMENT_3D ( 'NONE', #10132, #4186, #7588 ) ;
#8062 = CARTESIAN_POINT ( 'NONE',  ( -77.99999999999998579, 11.49999999999999645, -2.000000000000000000 ) ) ;
#8063 = DIRECTION ( 'NONE',  ( -0.000000000000000000, -0.000000000000000000, 1.000000000000000000 ) ) ;
#8064 = VERTEX_POINT ( 'NONE', #866 ) ;
#8065 = CARTESIAN_POINT ( 'NONE',  ( -61.99999999999998579, 10.43750000000000000, 2.500000000000002665 ) ) ;
#8066 = EDGE_LOOP ( 'NONE', ( #1669, #9940, #7792, #5347 ) ) ;
#8067 = UNCERTAINTY_MEASURE_WITH_UNIT (LENGTH_MEASURE( 1.000000000000000082E-05 ), #6073, 'distance_accuracy_value', 'NONE');
#8068 = CARTESIAN_POINT ( 'NONE',  ( -61.99999999999998579, 12.65624999931720396, 2.500000000000002665 ) ) ;
#8069 = CARTESIAN_POINT ( 'NONE',  ( -62.99999999999998579, 10.14583333333333393, 2.077350269189627952 ) ) ;
#8070 = CARTESIAN_POINT ( 'NONE',  ( -104.9999999999999289, -7.999999999999994671, -2.000000000000000000 ) ) ;
#8071 = CARTESIAN_POINT ( 'NONE',  ( -149.9999999999999716, -8.000000000000000000, 3.000000000000000000 ) ) ;
#8072 = LINE ( 'NONE', #5261, #10794 ) ;
#8073 = EDGE_CURVE ( 'NONE', #7434, #3822, #5190, .T. ) ;
#8074 = CARTESIAN_POINT ( 'NONE',  ( -61.99999999999998579, 9.765624999658600203, 2.498450539062049724 ) ) ;
#8075 = CARTESIAN_POINT ( 'NONE',  ( -62.26794919243111082, 11.39508544963257108, 2.500000000000003109 ) ) ;
#8076 = CARTESIAN_POINT ( 'NONE',  ( -61.73205080756886076, 15.41741454900183328, 2.500000000000003109 ) ) ;
#8077 = CARTESIAN_POINT ( 'NONE',  ( -61.13531646874998415, 10.36979166632526805, 1.999225269531026417 ) ) ;
#8078 = EDGE_CURVE ( 'NONE', #8566, #41, #4193, .T. ) ;
#8079 = LINE ( 'NONE', #7064, #10316 ) ;
#8080 = ORIENTED_EDGE ( 'NONE', *, *, #9014, .F. ) ;
#8081 = DIRECTION ( 'NONE',  ( 0.000000000000000000, -0.000000000000000000, 1.000000000000000000 ) ) ;
#8082 = UNCERTAINTY_MEASURE_WITH_UNIT (LENGTH_MEASURE( 1.000000000000000082E-05 ), #7930, 'distance_accuracy_value', 'NONE');
#8083 = CARTESIAN_POINT ( 'NONE',  ( -61.99999999999998579, 8.406249999317203958, 2.500000000000003109 ) ) ;
#8084 = EDGE_LOOP ( 'NONE', ( #4050, #1335, #2421, #1536 ) ) ;
#8085 = CARTESIAN_POINT ( 'NONE',  ( -61.49999999999998579, 15.70833333333333037, 2.366025403784441927 ) ) ;
#8086 = CARTESIAN_POINT ( 'NONE',  ( -62.86468353124998032, 11.93229166632526628, 1.000774730468978246 ) ) ;
#8087 = CARTESIAN_POINT ( 'NONE',  ( -61.13531646874997705, 10.30729166632526983, 1.999225269531026417 ) ) ;
#8088 = ORIENTED_EDGE ( 'NONE', *, *, #2466, .F. ) ;
#8089 = CARTESIAN_POINT ( 'NONE',  ( -37.99999999999999289, -14.00000000000000888, 3.999999999999999112 ) ) ;
#8090 = CARTESIAN_POINT ( 'NONE',  ( -62.86468353124999453, 11.51562499965860020, 1.500000000000002220 ) ) ;
#8091 = APPLICATION_PROTOCOL_DEFINITION ( 'draft international standard', 'automotive_design', 1998, #1660 ) ;
#8092 = CARTESIAN_POINT ( 'NONE',  ( -62.86468353124999453, 15.45312499965860020, 1.500000000000002220 ) ) ;
#8093 = CARTESIAN_POINT ( 'NONE',  ( -62.49999999999998579, 14.88541666598386826, 2.366025403784441483 ) ) ;
#8094 = CARTESIAN_POINT ( 'NONE',  ( -57.99999999999998579, -10.00000000000001066, -0.1418111474832477736 ) ) ;
#8095 = ORIENTED_EDGE ( 'NONE', *, *, #6549, .F. ) ;
#8096 = DIRECTION ( 'NONE',  ( 0.000000000000000000, 0.000000000000000000, 1.000000000000000000 ) ) ;
#8097 = VERTEX_POINT ( 'NONE', #7544 ) ;
#8098 = ADVANCED_FACE ( 'NONE', ( #6822 ), #2613, .T. ) ;
#8099 = CARTESIAN_POINT ( 'NONE',  ( -62.43234176562498305, 12.66145833299193413, 0.7511620957034662593 ) ) ;
#8100 = CARTESIAN_POINT ( 'NONE',  ( -62.86468353124998032, 8.682291666325268054, 1.000774730468978246 ) ) ;
#8101 = CARTESIAN_POINT ( 'NONE',  ( -61.99999999999997868, 10.65624999931720218, 2.500000000000002665 ) ) ;
#8102 = ORIENTED_EDGE ( 'NONE', *, *, #6750, .F. ) ;
#8103 = CARTESIAN_POINT ( 'NONE',  ( -62.49999999999998579, 12.33333333333333393, 0.6339745962155627357 ) ) ;
#8104 = CARTESIAN_POINT ( 'NONE',  ( -62.26794919243111082, 11.14508544963257286, 2.500000000000003109 ) ) ;
#8105 = CARTESIAN_POINT ( 'NONE',  ( -61.99999999999998579, 14.40624999931720218, 2.500000000000002665 ) ) ;
#8106 = CARTESIAN_POINT ( 'NONE',  ( -62.49999999999998579, 10.80208333265053611, 0.6339745962155627357 ) ) ;
#8107 = EDGE_LOOP ( 'NONE', ( #3683, #9678, #7960, #6438 ) ) ;
#8108 = CARTESIAN_POINT ( 'NONE',  ( -37.99999999999999289, -14.00000000000000888, 5.000000000000000000 ) ) ;
#8109 = CARTESIAN_POINT ( 'NONE',  ( -62.86468353124998032, 12.18229166632526805, 1.000774730468978246 ) ) ;
#8110 = VERTEX_POINT ( 'NONE', #6710 ) ;
#8111 = CARTESIAN_POINT ( 'NONE',  ( -61.56765823437498852, 11.59895833299193590, 2.248837904296538515 ) ) ;
#8112 = CARTESIAN_POINT ( 'NONE',  ( -79.09999999999998010, 11.49999999999999645, -2.000000000000000000 ) ) ;
#8113 = EDGE_CURVE ( 'NONE', #8064, #3822, #1597, .T. ) ;
#8114 = B_SPLINE_CURVE_WITH_KNOTS ( 'NONE', 3,
 ( #10950, #9136, #9243, #4956, #3339, #1684 ),
 .UNSPECIFIED., .F., .F.,
 ( 4, 2, 4 ),
 ( 0.003191392849877886743, 0.003612977948258624256, 0.004034563046639362202 ),
 .UNSPECIFIED. ) ;
#8115 = CARTESIAN_POINT ( 'NONE',  ( -62.43234176562499016, 15.55729166632526628, 2.248837904296538071 ) ) ;
#8116 = CARTESIAN_POINT ( 'NONE',  ( -61.49999999999998579, 9.010416665983868256, 0.6339745962155628467 ) ) ;
#8117 = ORIENTED_EDGE ( 'NONE', *, *, #6408, .F. ) ;
#8118 = CARTESIAN_POINT ( 'NONE',  ( -62.99999999999998579, 11.14583333333333393, 2.077350269189627952 ) ) ;
#8119 = ORIENTED_EDGE ( 'NONE', *, *, #8038, .T. ) ;
#8120 = CARTESIAN_POINT ( 'NONE',  ( -114.9999999999999289, -7.999999999999998224, 5.000000000000004441 ) ) ;
#8121 = CARTESIAN_POINT ( 'NONE',  ( -60.99999999999998579, 9.729166666666667851, 2.077350269189628840 ) ) ;
#8122 = CARTESIAN_POINT ( 'NONE',  ( -76.89999999999999147, 11.49999999999999645, -2.000000000000000000 ) ) ;
#8123 = CARTESIAN_POINT ( 'NONE',  ( -60.99999999999998579, 12.02083333333333215, 0.9226497308103762673 ) ) ;
#8124 = CARTESIAN_POINT ( 'NONE',  ( -61.13531646874998415, 10.59895833299193413, 1.000774730468978468 ) ) ;
#8125 = CARTESIAN_POINT ( 'NONE',  ( -61.99999999999998579, 8.281249999317203958, 0.3452994616207497591 ) ) ;
#8126 = CARTESIAN_POINT ( 'NONE',  ( -61.56765823437498852, 12.34895833299193413, 2.248837904296538515 ) ) ;
#8127 = CARTESIAN_POINT ( 'NONE',  ( -61.99999999999998579, 12.65624999931720396, 2.500000000000002665 ) ) ;
#8128 = EDGE_LOOP ( 'NONE', ( #10315, #3232 ) ) ;
#8129 = CARTESIAN_POINT ( 'NONE',  ( -76.99999999999998579, -11.50000000000000711, 5.000000000000000000 ) ) ;
#8130 = CARTESIAN_POINT ( 'NONE',  ( -62.99999999999998579, 9.104166666666666075, 0.9226497308103756012 ) ) ;
#8131 = MECHANICAL_DESIGN_GEOMETRIC_PRESENTATION_REPRESENTATION (  '', ( #1908 ), #2099 ) ;
#8132 = EDGE_CURVE ( 'NONE', #3822, #9355, #668, .T. ) ;
#8133 = EDGE_LOOP ( 'NONE', ( #4147, #5284, #812, #7828 ) ) ;
#8134 = CARTESIAN_POINT ( 'NONE',  ( -60.99999999999998579, 15.77083333333332860, 0.9226497308103762673 ) ) ;
#8135 = CARTESIAN_POINT ( 'NONE',  ( -61.56765823437498142, 13.61979166632526805, 0.7511620957034663704 ) ) ;
#8136 = EDGE_CURVE ( 'NONE', #6280, #1179, #4919, .T. ) ;
#8137 = CARTESIAN_POINT ( 'NONE',  ( -61.13531646874998415, 10.82812499965860020, 1.500000000000002220 ) ) ;
#8138 = CARTESIAN_POINT ( 'NONE',  ( -61.99999999999997868, 11.65624999931720218, 2.500000000000002665 ) ) ;
#8139 = EDGE_LOOP ( 'NONE', ( #3920, #2523, #10765, #9369 ) ) ;
#8140 = LINE ( 'NONE', #9962, #6172 ) ;
#8141 = CARTESIAN_POINT ( 'NONE',  ( -61.56765823437498142, 11.18229166632526805, 0.7511620957034663704 ) ) ;
#8142 = AXIS2_PLACEMENT_3D ( 'NONE', #9305, #965, #6921 ) ;
#8143 = DIRECTION ( 'NONE',  ( 0.000000000000000000, 0.000000000000000000, -1.000000000000000000 ) ) ;
#8144 = CYLINDRICAL_SURFACE ( 'NONE', #6719, 0.9999999999999981126 ) ;
#8145 = CARTESIAN_POINT ( 'NONE',  ( -62.49999999999998579, 15.30208333265053611, 0.6339745962155627357 ) ) ;
#8146 = DIRECTION ( 'NONE',  ( 0.000000000000000000, 0.000000000000000000, -1.000000000000000000 ) ) ;
#8147 = ORIENTED_EDGE ( 'NONE', *, *, #2709, .F. ) ;
#8148 =( LENGTH_UNIT ( ) NAMED_UNIT ( * ) SI_UNIT ( .MILLI., .METRE. ) );
#8149 = ORIENTED_EDGE ( 'NONE', *, *, #7089, .F. ) ;
#8150 = AXIS2_PLACEMENT_3D ( 'NONE', #4492, #2118, #8785 ) ;
#8151 = CARTESIAN_POINT ( 'NONE',  ( -61.99999999999999289, 13.51562499965860198, 2.498450539062049724 ) ) ;
#8152 = CARTESIAN_POINT ( 'NONE',  ( -61.13531646874998415, 9.348958332991935904, 1.000774730468978468 ) ) ;
#8153 = VECTOR ( 'NONE', #10044, 1000.000000000000000 ) ;
#8154 = DIRECTION ( 'NONE',  ( 0.000000000000000000, 1.000000000000000000, 0.000000000000000000 ) ) ;
#8155 = ORIENTED_EDGE ( 'NONE', *, *, #5061, .F. ) ;
#8156 = CARTESIAN_POINT ( 'NONE',  ( -62.49999999999998579, 12.83333333333333393, 0.6339745962155627357 ) ) ;
#8157 = CARTESIAN_POINT ( 'NONE',  ( -62.26794919243111082, 11.04241454900183150, 0.5000000000000013323 ) ) ;
#8158 = ADVANCED_FACE ( 'NONE', ( #8771 ), #378, .F. ) ;
#8159 = AXIS2_PLACEMENT_3D ( 'NONE', #4843, #7467, #8196 ) ;
#8160 = CARTESIAN_POINT ( 'NONE',  ( -60.99999999999998579, 10.94791666598386826, 2.077350269189628840 ) ) ;
#8161 = VECTOR ( 'NONE', #10330, 1000.000000000000000 ) ;
#8162 = CARTESIAN_POINT ( 'NONE',  ( -62.43234176562499016, 12.74479166632526805, 2.248837904296538071 ) ) ;
#8163 = CARTESIAN_POINT ( 'NONE',  ( 0.000000000000000000, -0.2499999999999997780, -1.312875263449798879 ) ) ;
#8164 = VECTOR ( 'NONE', #8428, 1000.000000000000000 ) ;
#8165 = ORIENTED_EDGE ( 'NONE', *, *, #9343, .T. ) ;
#8166 = CARTESIAN_POINT ( 'NONE',  ( -62.86468353124998032, 11.74479166632526628, 1.000774730468978246 ) ) ;
#8167 = CARTESIAN_POINT ( 'NONE',  ( -62.99999999999998579, 12.57291666598387003, 0.9226497308103756012 ) ) ;
#8168 = VECTOR ( 'NONE', #3938, 1000.000000000000000 ) ;
#8169 = CARTESIAN_POINT ( 'NONE',  ( -61.99999999999998579, 15.70312499965860198, 0.5015494609379544944 ) ) ;
#8170 = ORIENTED_EDGE ( 'NONE', *, *, #9835, .F. ) ;
#8171 = DIRECTION ( 'NONE',  ( -0.000000000000000000, -0.000000000000000000, -1.000000000000000000 ) ) ;
#8172 = STYLED_ITEM ( 'NONE', ( #7375 ), #6440 ) ;
#8173 = EDGE_LOOP ( 'NONE', ( #3749, #18, #7115, #122 ) ) ;
#8174 = DIRECTION ( 'NONE',  ( 0.000000000000000000, 1.065814103640150121E-14, 1.000000000000000000 ) ) ;
#8175 = CARTESIAN_POINT ( 'NONE',  ( -61.99999999999998579, 10.06249999999999822, 0.3452994616207497591 ) ) ;
#8176 = AXIS2_PLACEMENT_3D ( 'NONE', #4037, #8226, #5547 ) ;
#8177 = PLANE ( 'NONE',  #2210 ) ;
#8178 = DIRECTION ( 'NONE',  ( -0.000000000000000000, -0.000000000000000000, -1.000000000000000000 ) ) ;
#8179 = FACE_BOUND ( 'NONE', #464, .T. ) ;
#8180 = EDGE_CURVE ( 'NONE', #5034, #3952, #9773, .T. ) ;
#8181 = DIRECTION ( 'NONE',  ( 1.000000000000000000, 0.000000000000000000, 0.000000000000000000 ) ) ;
#8182 = CARTESIAN_POINT ( 'NONE',  ( -62.86468353124999453, 11.26562499965860020, 1.500000000000002220 ) ) ;
#8183 = CARTESIAN_POINT ( 'NONE',  ( -62.99999999999998579, 9.093749999317203958, 1.500000000000001998 ) ) ;
#8184 = ORIENTED_EDGE ( 'NONE', *, *, #3607, .F. ) ;
#8185 = DIRECTION ( 'NONE',  ( -0.000000000000000000, -1.000000000000000000, -0.000000000000000000 ) ) ;
#8186 = CARTESIAN_POINT ( 'NONE',  ( 0.000000000000000000, 0.2499999999999982792, -1.312875263449799323 ) ) ;
#8187 = EDGE_CURVE ( 'NONE', #8064, #4883, #7102, .T. ) ;
#8188 = EDGE_LOOP ( 'NONE', ( #8006, #2036, #6772, #4250 ) ) ;
#8189 = CARTESIAN_POINT ( 'NONE',  ( -60.99999999999998579, 14.19791666598386826, 2.077350269189628840 ) ) ;
#8190 = CARTESIAN_POINT ( 'NONE',  ( -61.56765823437498852, 13.28645833299193413, 2.248837904296538515 ) ) ;
#8191 = CARTESIAN_POINT ( 'NONE',  ( -62.86468353124998032, 9.682291666325266277, 1.000774730468978024 ) ) ;
#8192 = CARTESIAN_POINT ( 'NONE',  ( -62.99999999999998579, 8.125000000000000000, 1.500000000000001998 ) ) ;
#8193 = ORIENTED_EDGE ( 'NONE', *, *, #6090, .T. ) ;
#8194 = CARTESIAN_POINT ( 'NONE',  ( -62.26794919243110371, 8.292414549001831503, 0.4999999999999997780 ) ) ;
#8195 = CARTESIAN_POINT ( 'NONE',  ( -61.13531646874997705, 11.36979166632526628, 1.999225269531026417 ) ) ;
#8196 = DIRECTION ( 'NONE',  ( 0.000000000000000000, 0.000000000000000000, -1.000000000000000000 ) ) ;
#8197 = CARTESIAN_POINT ( 'NONE',  ( -62.99999999999998579, 15.32291666598387003, 0.9226497308103756012 ) ) ;
#8198 = CYLINDRICAL_SURFACE ( 'NONE', #8548, 1.000000000000000000 ) ;
#8199 = ORIENTED_EDGE ( 'NONE', *, *, #4849, .T. ) ;
#8200 = CARTESIAN_POINT ( 'NONE',  ( 195.0000000000000000, -4.336808689942017736E-16, 2.000000000000000000 ) ) ;
#8201 = DIRECTION ( 'NONE',  ( 0.000000000000000000, 1.000000000000000000, 0.000000000000000000 ) ) ;
#8202 = CARTESIAN_POINT ( 'NONE',  ( -61.99999999999999289, 14.26562499965860020, 2.498450539062049724 ) ) ;
#8203 = CARTESIAN_POINT ( 'NONE',  ( -61.13531646874998415, 10.34895833299193413, 1.000774730468978468 ) ) ;
#8204 = CARTESIAN_POINT ( 'NONE',  ( -61.99999999999998579, 13.56249999999999822, 0.5000000000000013323 ) ) ;
#8205 = VERTEX_POINT ( 'NONE', #3587 ) ;
#8206 = CARTESIAN_POINT ( 'NONE',  ( -62.49999999999998579, 13.41666666666666785, 2.366025403784441483 ) ) ;
#8207 = CARTESIAN_POINT ( 'NONE',  ( -62.49999999999998579, 13.38541666598387003, 2.366025403784441483 ) ) ;
#8208 =( LENGTH_UNIT ( ) NAMED_UNIT ( * ) SI_UNIT ( .MILLI., .METRE. ) );
#8209 = EDGE_CURVE ( 'NONE', #9658, #4192, #4531, .T. ) ;
#8210 = CARTESIAN_POINT ( 'NONE',  ( -62.99999999999998579, 11.59374999931720218, 1.500000000000001998 ) ) ;
#8211 = AXIS2_PLACEMENT_3D ( 'NONE', #2733, #6116, #5054 ) ;
#8212 = EDGE_CURVE ( 'NONE', #2941, #5442, #10060, .T. ) ;
#8213 = DIRECTION ( 'NONE',  ( -0.000000000000000000, -1.000000000000000000, -0.000000000000000000 ) ) ;
#8214 = CARTESIAN_POINT ( 'NONE',  ( -61.56765823437498852, 14.28645833299193413, 2.248837904296538515 ) ) ;
#8215 =( NAMED_UNIT ( * ) PLANE_ANGLE_UNIT ( ) SI_UNIT ( $, .RADIAN. ) );
#8216 =( BOUNDED_CURVE ( )  B_SPLINE_CURVE ( 2, ( #8065, #1102, #3833, #5372, #2948, #8780, #2112, #7944, #4430 ),
 .UNSPECIFIED., .F., .T. ) 
 B_SPLINE_CURVE_WITH_KNOTS ( ( 3, 2, 2, 2, 3 ),
 ( 0.3046875000000000000, 0.3072916666666666852, 0.3125000000000000000, 0.3177083333333333148, 0.3203125000000000000 ),
 .UNSPECIFIED. ) 
 CURVE ( )  GEOMETRIC_REPRESENTATION_ITEM ( )  RATIONAL_B_SPLINE_CURVE ( ( 0.9330127018922194093, 0.9330127018922194093, 1.000000000000000000, 0.8660254037844387076, 1.000000000000000000, 0.8660254037844387076, 1.000000000000000000, 0.9330127018922194093, 0.9330127018922194093 ) ) 
 REPRESENTATION_ITEM ( '' )  );
#8217 = ORIENTED_EDGE ( 'NONE', *, *, #7525, .T. ) ;
#8218 = AXIS2_PLACEMENT_3D ( 'NONE', #6465, #404, #4500 ) ;
#8219 = CIRCLE ( 'NONE', #3405, 1.928074011315806136 ) ;
#8220 = CARTESIAN_POINT ( 'NONE',  ( -61.99999999999998579, 12.07812499965860020, 2.498450539062049724 ) ) ;
#8221 = CARTESIAN_POINT ( 'NONE',  ( -120.0000000000000000, 14.99999999999998579, 0.000000000000000000 ) ) ;
#8222 = PRODUCT_DEFINITION_SHAPE ( 'NONE', 'NONE',  #10791 ) ;
#8223 = FACE_OUTER_BOUND ( 'NONE', #10866, .T. ) ;
#8224 = ORIENTED_EDGE ( 'NONE', *, *, #9254, .F. ) ;
#8225 = CONICAL_SURFACE ( 'NONE', #8048, 1.000000000000000888, 1.029744259999999967 ) ;
#8226 = DIRECTION ( 'NONE',  ( 1.000000000000000000, 0.000000000000000000, 0.000000000000000000 ) ) ;
#8227 = AXIS2_PLACEMENT_3D ( 'NONE', #10769, #10825, #5766 ) ;
#8228 = EDGE_CURVE ( 'NONE', #8833, #9827, #1396, .T. ) ;
#8229 = VERTEX_POINT ( 'NONE', #9594 ) ;
#8230 = CARTESIAN_POINT ( 'NONE',  ( -61.73205080756886787, 8.770085449632572860, 0.5000000000000006661 ) ) ;
#8231 = CARTESIAN_POINT ( 'NONE',  ( -62.99999999999998579, 9.875000000000000000, 1.500000000000001998 ) ) ;
#8232 = CARTESIAN_POINT ( 'NONE',  ( 0.000000000000000000, 0.2499999999999998335, 1.312875263449799101 ) ) ;
#8233 = CYLINDRICAL_SURFACE ( 'NONE', #8314, 0.9999999999999981126 ) ;
#8234 = CARTESIAN_POINT ( 'NONE',  ( -61.49999999999998579, 15.51041666598387003, 0.6339745962155628467 ) ) ;
#8235 = CARTESIAN_POINT ( 'NONE',  ( -61.99999999999998579, 12.07812499965860020, 2.498450539062049724 ) ) ;
#8236 = CARTESIAN_POINT ( 'NONE',  ( -62.26794919243112503, 10.67633545031536890, 2.500000000000000000 ) ) ;
#8237 = ORIENTED_EDGE ( 'NONE', *, *, #5422, .T. ) ;
#8238 = LINE ( 'NONE', #6467, #710 ) ;
#8239 = CARTESIAN_POINT ( 'NONE',  ( -61.99999999999998579, 16.00000000000000000, 1.500000000000002220 ) ) ;
#8240 = VECTOR ( 'NONE', #1445, 1000.000000000000000 ) ;
#8241 = EDGE_CURVE ( 'NONE', #2188, #3431, #8712, .T. ) ;
#8242 = ORIENTED_EDGE ( 'NONE', *, *, #1384, .T. ) ;
#8243 = LINE ( 'NONE', #2238, #6960 ) ;
#8244 = CARTESIAN_POINT ( 'NONE',  ( -61.13531646874998415, 13.59895833299193413, 1.000774730468978468 ) ) ;
#8245 = CARTESIAN_POINT ( 'NONE',  ( -62.43234176562499016, 9.744791666325268054, 2.248837904296538071 ) ) ;
#8246 = DIRECTION ( 'NONE',  ( 0.000000000000000000, 0.000000000000000000, 1.000000000000000000 ) ) ;
#8247 = CARTESIAN_POINT ( 'NONE',  ( -62.26794919243110371, 8.395085449632571084, 2.500000000000000888 ) ) ;
#8248 = CARTESIAN_POINT ( 'NONE',  ( -62.43234176562498305, 11.97395833299193413, 0.7511620957034662593 ) ) ;
#8249 = CARTESIAN_POINT ( 'NONE',  ( -61.99999999999998579, 8.140624999658601979, 0.5015494609379544944 ) ) ;
#8250 = SHAPE_DEFINITION_REPRESENTATION ( #1831, #2047 ) ;
#8251 = CARTESIAN_POINT ( 'NONE',  ( -62.99999999999998579, 13.59374999931720218, 1.500000000000001998 ) ) ;
#8252 = EDGE_CURVE ( 'NONE', #4539, #10433, #9709, .T. ) ;
#8253 = CARTESIAN_POINT ( 'NONE',  ( -61.99999999999998579, 8.453124999658601979, 0.5015494609379544944 ) ) ;
#8254 = CARTESIAN_POINT ( 'NONE',  ( -37.99999999999999289, -14.00000000000000888, 3.999999999999999112 ) ) ;
#8255 = VERTEX_POINT ( 'NONE', #7158 ) ;
#8256 = DIRECTION ( 'NONE',  ( 0.000000000000000000, 0.000000000000000000, 1.000000000000000000 ) ) ;
#8257 = CARTESIAN_POINT ( 'NONE',  ( 0.000000000000000000, 2.310008073021392973E-16, 1.886264737416298631 ) ) ;
#8258 = CARTESIAN_POINT ( 'NONE',  ( -62.86468353124999453, 13.72395833299193590, 1.999225269531025750 ) ) ;
#8259 = CARTESIAN_POINT ( 'NONE',  ( -61.99999999999998579, 9.765624999658600203, 2.498450539062049724 ) ) ;
#8260 = CARTESIAN_POINT ( 'NONE',  ( -49.99999999999998579, 8.000000000000000000, 0.000000000000000000 ) ) ;
#8261 = VERTEX_POINT ( 'NONE', #8823 ) ;
#8262 = CARTESIAN_POINT ( 'NONE',  ( -62.99999999999998579, 14.37499999999999822, 1.500000000000001998 ) ) ;
#8263 = CARTESIAN_POINT ( 'NONE',  ( -62.49999999999998579, 11.05208333265053611, 0.6339745962155627357 ) ) ;
#8264 =( LENGTH_UNIT ( ) NAMED_UNIT ( * ) SI_UNIT ( .MILLI., .METRE. ) );
#8265 = CARTESIAN_POINT ( 'NONE',  ( -61.49999999999998579, 12.01041666598387003, 0.6339745962155628467 ) ) ;
#8266 = CARTESIAN_POINT ( 'NONE',  ( -62.86468353124998742, 14.47395833299193413, 1.999225269531025972 ) ) ;
#8267 = ORIENTED_EDGE ( 'NONE', *, *, #5763, .T. ) ;
#8268 = ADVANCED_FACE ( 'NONE', ( #8882 ), #9534, .T. ) ;
#8269 = CARTESIAN_POINT ( 'NONE',  ( -62.43234176562499016, 11.55729166632526805, 2.248837904296538071 ) ) ;
#8270 = DIRECTION ( 'NONE',  ( -1.000000000000000000, 0.000000000000000000, 0.000000000000000000 ) ) ;
#8271 = CARTESIAN_POINT ( 'NONE',  ( -61.13531646874998415, 16.14062499965860198, 1.500000000000002220 ) ) ;
#8272 = ORIENTED_EDGE ( 'NONE', *, *, #3057, .T. ) ;
#8273 = FACE_OUTER_BOUND ( 'NONE', #3472, .T. ) ;
#8274 =( BOUNDED_CURVE ( )  B_SPLINE_CURVE ( 2, ( #9905, #5731, #10839, #9125, #4112, #2295, #3223, #5680, #1512 ),
 .UNSPECIFIED., .F., .T. ) 
 B_SPLINE_CURVE_WITH_KNOTS ( ( 3, 2, 2, 2, 3 ),
 ( 0.8046875000000000000, 0.8072916666666666297, 0.8125000000000000000, 0.8177083333333333703, 0.8203125000000000000 ),
 .UNSPECIFIED. ) 
 CURVE ( )  GEOMETRIC_REPRESENTATION_ITEM ( )  RATIONAL_B_SPLINE_CURVE ( ( 0.9330127018922194093, 0.9330127018922194093, 1.000000000000000000, 0.8660254037844387076, 1.000000000000000000, 0.8660254037844387076, 1.000000000000000000, 0.9330127018922194093, 0.9330127018922194093 ) ) 
 REPRESENTATION_ITEM ( '' )  );
#8275 = ORIENTED_EDGE ( 'NONE', *, *, #1317, .F. ) ;
#8276 = DIRECTION ( 'NONE',  ( -1.000000000000000000, 0.000000000000000000, 0.000000000000000000 ) ) ;
#8277 = CARTESIAN_POINT ( 'NONE',  ( -61.49999999999998579, 9.958333333333332149, 2.366025403784441927 ) ) ;
#8278 = PLANE ( 'NONE',  #10431 ) ;
#8279 = CARTESIAN_POINT ( 'NONE',  ( -60.99999999999998579, 12.27083333333333570, 0.9226497308103762673 ) ) ;
#8280 = CARTESIAN_POINT ( 'NONE',  ( 150.0000000000000284, -8.000000000000000000, 3.000000000000000000 ) ) ;
#8281 = ADVANCED_FACE ( 'NONE', ( #10419 ), #5244, .T. ) ;
#8282 = CARTESIAN_POINT ( 'NONE',  ( -62.86468353124998742, 11.28645833299193590, 1.999225269531025972 ) ) ;
#8283 = CARTESIAN_POINT ( 'NONE',  ( -61.99999999999998579, 14.53124999931720041, 0.5000000000000013323 ) ) ;
#8284 = ORIENTED_EDGE ( 'NONE', *, *, #6463, .T. ) ;
#8285 = CARTESIAN_POINT ( 'NONE',  ( -57.99999999999998579, -10.00000000000001066, 5.282956808509874826E-15 ) ) ;
#8286 = ORIENTED_EDGE ( 'NONE', *, *, #7358, .F. ) ;
#8287 = DIRECTION ( 'NONE',  ( 0.000000000000000000, 0.000000000000000000, -1.000000000000000000 ) ) ;
#8288 = CARTESIAN_POINT ( 'NONE',  ( -61.99999999999998579, 13.39062499965860020, 0.5015494609379544944 ) ) ;
#8289 = DIRECTION ( 'NONE',  ( 1.000000000000000000, -1.734723475976805517E-15, 0.000000000000000000 ) ) ;
#8290 = DIRECTION ( 'NONE',  ( -0.000000000000000000, -1.000000000000000000, -0.000000000000000000 ) ) ;
#8291 = CARTESIAN_POINT ( 'NONE',  ( -61.13531646874997705, 13.16145833299193413, 1.000774730468978468 ) ) ;
#8292 = CARTESIAN_POINT ( 'NONE',  ( -61.13531646874998415, 15.16145833299193590, 1.000774730468978468 ) ) ;
#8293 = CARTESIAN_POINT ( 'NONE',  ( -61.99999999999998579, 13.90624999931720218, 2.500000000000002665 ) ) ;
#8294 = CARTESIAN_POINT ( 'NONE',  ( -62.26794919243111082, 13.54241454900183150, 0.5000000000000013323 ) ) ;
#8295 = CARTESIAN_POINT ( 'NONE',  ( -61.49999999999998579, 16.01041666598386826, 0.6339745962155628467 ) ) ;
#8296 = DIRECTION ( 'NONE',  ( -0.000000000000000000, 0.000000000000000000, -1.000000000000000000 ) ) ;
#8297 = VERTEX_POINT ( 'NONE', #2706 ) ;
#8298 = FACE_OUTER_BOUND ( 'NONE', #5967, .T. ) ;
#8299 = CARTESIAN_POINT ( 'NONE',  ( -61.99999999999999289, 14.14062499965860198, 0.5015494609379544944 ) ) ;
#8300 = CARTESIAN_POINT ( 'NONE',  ( -61.99999999999998579, 9.640624999658600203, 0.5015494609379544944 ) ) ;
#8301 = CIRCLE ( 'NONE', #7238, 1.928074011315806136 ) ;
#8302 = CARTESIAN_POINT ( 'NONE',  ( -61.13531646874998415, 16.14062499965860198, 1.500000000000002220 ) ) ;
#8303 = FACE_OUTER_BOUND ( 'NONE', #7239, .T. ) ;
#8304 = ORIENTED_EDGE ( 'NONE', *, *, #10418, .T. ) ;
#8305 = CARTESIAN_POINT ( 'NONE',  ( -61.49999999999998579, 13.70833333333333215, 2.366025403784441927 ) ) ;
#8306 = PRODUCT_DEFINITION_SHAPE ( 'NONE', 'NONE',  #10986 ) ;
#8307 = DIRECTION ( 'NONE',  ( 1.000000000000000000, 3.965082230804130220E-16, -0.000000000000000000 ) ) ;
#8308 = CARTESIAN_POINT ( 'NONE',  ( -62.99999999999998579, 11.57291666598387003, 0.9226497308103756012 ) ) ;
#8309 = CARTESIAN_POINT ( 'NONE',  ( -77.99999999999998579, 0.000000000000000000, 13.00000000000000178 ) ) ;
#8310 = VECTOR ( 'NONE', #5599, 1000.000000000000000 ) ;
#8311 = CARTESIAN_POINT ( 'NONE',  ( -62.86468353124998032, 13.68229166632526983, 1.000774730468978246 ) ) ;
#8312 = EDGE_CURVE ( 'NONE', #3615, #10295, #4429, .T. ) ;
#8313 = ORIENTED_EDGE ( 'NONE', *, *, #1429, .F. ) ;
#8314 = AXIS2_PLACEMENT_3D ( 'NONE', #6509, #9162, #9996 ) ;
#8315 = CARTESIAN_POINT ( 'NONE',  ( -61.13531646874998415, 11.91145833299193413, 1.000774730468978468 ) ) ;
#8316 = DIRECTION ( 'NONE',  ( 0.000000000000000000, 0.000000000000000000, -1.000000000000000000 ) ) ;
#8317 = VECTOR ( 'NONE', #2534, 1000.000000000000000 ) ;
#8318 = CARTESIAN_POINT ( 'NONE',  ( 0.05007509226404533581, 0.2499999999999982236, 1.595201548406556480 ) ) ;
#8319 = ORIENTED_EDGE ( 'NONE', *, *, #8995, .T. ) ;
#8320 = CARTESIAN_POINT ( 'NONE',  ( -61.99999999999998579, 14.99999999999998579, 2.500000000000003109 ) ) ;
#8321 = VECTOR ( 'NONE', #6841, 1000.000000000000000 ) ;
#8322 = EDGE_CURVE ( 'NONE', #8835, #3864, #8301, .T. ) ;
#8323 = VERTEX_POINT ( 'NONE', #3098 ) ;
#8324 = CARTESIAN_POINT ( 'NONE',  ( -61.49999999999998579, 9.510416665983870033, 0.6339745962155628467 ) ) ;
#8325 = CARTESIAN_POINT ( 'NONE',  ( -62.49999999999998579, 11.08333333333333393, 0.6339745962155627357 ) ) ;
#8326 =( REPRESENTATION_RELATIONSHIP ('NONE','NONE', #560, #2752 ) REPRESENTATION_RELATIONSHIP_WITH_TRANSFORMATION ( #1468 )SHAPE_REPRESENTATION_RELATIONSHIP( ) );
#8327 = CARTESIAN_POINT ( 'NONE',  ( -60.99999999999998579, 14.96874999931720218, 1.500000000000002220 ) ) ;
#8328 = CARTESIAN_POINT ( 'NONE',  ( -60.99999999999998579, 8.229166666666667851, 2.077350269189628840 ) ) ;
#8329 = AXIS2_PLACEMENT_3D ( 'NONE', #6687, #588, #739 ) ;
#8330 = CARTESIAN_POINT ( 'NONE',  ( -61.49999999999998579, 9.177083332650536107, 2.366025403784441927 ) ) ;
#8331 = ADVANCED_FACE ( 'NONE', ( #3047 ), #6494, .F. ) ;
#8332 = CARTESIAN_POINT ( 'NONE',  ( -61.13531646874998415, 11.91145833299193413, 1.000774730468978468 ) ) ;
#8333 = AXIS2_PLACEMENT_3D ( 'NONE', #9459, #7021, #1909 ) ;
#8334 = CARTESIAN_POINT ( 'NONE',  ( -62.99999999999998579, 14.59374999931720218, 1.500000000000001998 ) ) ;
#8335 = VERTEX_POINT ( 'NONE', #7320 ) ;
#8336 =( BOUNDED_CURVE ( )  B_SPLINE_CURVE ( 2, ( #8875, #194, #1263, #434, #3818, #3579, #10297 ),
 .UNSPECIFIED., .F., .T. ) 
 B_SPLINE_CURVE_WITH_KNOTS ( ( 3, 2, 2, 3 ),
 ( 0.9609375000000000000, 0.9635416666666666297, 0.9687500000000000000, 0.9725886266600324292 ),
 .UNSPECIFIED. ) 
 CURVE ( )  GEOMETRIC_REPRESENTATION_ITEM ( )  RATIONAL_B_SPLINE_CURVE ( ( 0.9330127018922194093, 0.9330127018922194093, 1.000000000000000000, 0.8660254037844387076, 1.000000000000000000, 0.9012585362943751344, 0.9480652127606670199 ) ) 
 REPRESENTATION_ITEM ( '' )  );
#8337 = CARTESIAN_POINT ( 'NONE',  ( -62.49999999999998579, 15.41666666666666607, 2.366025403784441483 ) ) ;
#8338 = EDGE_CURVE ( 'NONE', #6686, #3194, #215, .T. ) ;
#8339 = AXIS2_PLACEMENT_3D ( 'NONE', #9794, #2850, #2186 ) ;
#8340 = ORIENTED_EDGE ( 'NONE', *, *, #10973, .F. ) ;
#8341 = CARTESIAN_POINT ( 'NONE',  ( -61.99999999999998579, 13.65624999931720218, 2.500000000000002665 ) ) ;
#8342 = EDGE_CURVE ( 'NONE', #8888, #2070, #2524, .T. ) ;
#8343 = CARTESIAN_POINT ( 'NONE',  ( -62.43234176562499016, 13.99479166632526805, 2.248837904296538071 ) ) ;
#8344 = CARTESIAN_POINT ( 'NONE',  ( 140.0000000000000284, -8.000000000000000000, 6.000000000000000000 ) ) ;
#8345 = CARTESIAN_POINT ( 'NONE',  ( -61.13531646874998415, 13.66145833299193590, 1.000774730468978468 ) ) ;
#8346 = PLANE ( 'NONE',  #6180 ) ;
#8347 = DIRECTION ( 'NONE',  ( -0.000000000000000000, -0.000000000000000000, 1.000000000000000000 ) ) ;
#8348 = PRODUCT_DEFINITION_CONTEXT ( 'detailed design', #10377, 'design' ) ;
#8349 = CARTESIAN_POINT ( 'NONE',  ( -61.13531646874997705, 12.61979166632526805, 1.999225269531026417 ) ) ;
#8350 = CARTESIAN_POINT ( 'NONE',  ( -61.56765823437498142, 15.68229166632526628, 0.7511620957034663704 ) ) ;
#8351 = LINE ( 'NONE', #4118, #862 ) ;
#8352 = FACE_OUTER_BOUND ( 'NONE', #612, .T. ) ;
#8353 = CARTESIAN_POINT ( 'NONE',  ( -62.99999999999998579, 16.09374999931720396, 1.500000000000001998 ) ) ;
#8354 = CARTESIAN_POINT ( 'NONE',  ( -62.26794919243111082, 10.42633545031537246, 2.500000000000003109 ) ) ;
#8355 = ORIENTED_EDGE ( 'NONE', *, *, #5371, .T. ) ;
#8356 = DIRECTION ( 'NONE',  ( -0.000000000000000000, 0.000000000000000000, 1.000000000000000000 ) ) ;
#8357 = CARTESIAN_POINT ( 'NONE',  ( -61.99999999999998579, 12.56249999999999822, 0.5000000000000013323 ) ) ;
#8358 = CARTESIAN_POINT ( 'NONE',  ( -62.86468353124998032, 14.43229166632526983, 1.000774730468978024 ) ) ;
#8359 = ADVANCED_FACE ( 'NONE', ( #7378 ), #4808, .F. ) ;
#8360 = CARTESIAN_POINT ( 'NONE',  ( -61.13531646874998415, 9.598958332991934128, 1.000774730468978468 ) ) ;
#8361 = CARTESIAN_POINT ( 'NONE',  ( -61.13531646874997705, 15.66145833299193590, 1.000774730468978468 ) ) ;
#8362 = DIRECTION ( 'NONE',  ( 1.000000000000000000, 0.000000000000000000, -0.000000000000000000 ) ) ;
#8363 = ORIENTED_EDGE ( 'NONE', *, *, #9314, .F. ) ;
#8364 = CARTESIAN_POINT ( 'NONE',  ( -60.99999999999998579, 13.52083333333333215, 0.9226497308103762673 ) ) ;
#8365 = CARTESIAN_POINT ( 'NONE',  ( -61.13531646874998415, 9.390624999658600203, 1.500000000000002220 ) ) ;
#8366 = UNCERTAINTY_MEASURE_WITH_UNIT (LENGTH_MEASURE( 1.000000000000000082E-05 ), #2040, 'distance_accuracy_value', 'NONE');
#8367 = CARTESIAN_POINT ( 'NONE',  ( -61.49999999999998579, 12.17708333265053611, 2.366025403784441927 ) ) ;
#8368 = CARTESIAN_POINT ( 'NONE',  ( -25.39999999999996305, 0.000000000000000000, 0.000000000000000000 ) ) ;
#8369 = CARTESIAN_POINT ( 'NONE',  ( -62.86468353124998742, 13.72395833299193413, 1.999225269531025972 ) ) ;
#8370 = SURFACE_SIDE_STYLE ('',( #5805 ) ) ;
#8371 = ADVANCED_FACE ( 'NONE', ( #9768 ), #10592, .T. ) ;
#8372 = VERTEX_POINT ( 'NONE', #10757 ) ;
#8373 = CARTESIAN_POINT ( 'NONE',  ( -61.99999999999998579, 13.07812499965860198, 2.498450539062049724 ) ) ;
#8374 = CARTESIAN_POINT ( 'NONE',  ( -114.9999999999999289, -7.999999999999998224, -2.000000000000000000 ) ) ;
#8375 = EDGE_CURVE ( 'NONE', #3158, #7302, #6876, .T. ) ;
#8376 = CARTESIAN_POINT ( 'NONE',  ( -61.99999999999998579, 13.78124999931720218, 0.5000000000000013323 ) ) ;
#8377 = EDGE_LOOP ( 'NONE', ( #10416, #5914, #10916, #3424 ) ) ;
#8378 = DIRECTION ( 'NONE',  ( -1.000000000000000000, 0.000000000000000000, 0.000000000000000000 ) ) ;
#8379 = CIRCLE ( 'NONE', #9432, 1.928074011315806136 ) ;
#8380 = VECTOR ( 'NONE', #5642, 1000.000000000000000 ) ;
#8381 = VERTEX_POINT ( 'NONE', #4702 ) ;
#8382 = CARTESIAN_POINT ( 'NONE',  ( -62.49999999999998579, 11.58333333333333393, 0.6339745962155627357 ) ) ;
#8383 = EDGE_LOOP ( 'NONE', ( #4688, #4219, #5773, #10176 ) ) ;
#8384 = DIRECTION ( 'NONE',  ( 3.965082230804130220E-16, -1.000000000000000000, 0.000000000000000000 ) ) ;
#8385 = CARTESIAN_POINT ( 'NONE',  ( -62.49999999999998579, 13.88541666598387003, 2.366025403784441483 ) ) ;
#8386 =( GEOMETRIC_REPRESENTATION_CONTEXT ( 3 ) GLOBAL_UNCERTAINTY_ASSIGNED_CONTEXT ( ( #1170 ) ) GLOBAL_UNIT_ASSIGNED_CONTEXT ( ( #8148, #1369, #2978 ) ) REPRESENTATION_CONTEXT ( 'NONE', 'WORKASPACE' ) );
#8387 = VECTOR ( 'NONE', #7754, 1000.000000000000000 ) ;
#8388 = CARTESIAN_POINT ( 'NONE',  ( -62.86468353124998742, 13.28645833299193413, 1.999225269531025972 ) ) ;
#8389 = ORIENTED_EDGE ( 'NONE', *, *, #8338, .T. ) ;
#8390 = PLANE ( 'NONE',  #3719 ) ;
#8391 = ORIENTED_EDGE ( 'NONE', *, *, #10648, .T. ) ;
#8392 = AXIS2_PLACEMENT_3D ( 'NONE', #3514, #3569, #6075 ) ;
#8393 = CARTESIAN_POINT ( 'NONE',  ( -61.73205080756886076, 13.27008544963257286, 0.5000000000000014433 ) ) ;
#8394 = EDGE_CURVE ( 'NONE', #4184, #4203, #3868, .T. ) ;
#8395 = CARTESIAN_POINT ( 'NONE',  ( -61.56765823437498852, 15.78645833299193590, 2.248837904296538515 ) ) ;
#8396 = CARTESIAN_POINT ( 'NONE',  ( -62.99999999999998579, 11.87500000000000000, 1.500000000000001998 ) ) ;
#8397 = DIRECTION ( 'NONE',  ( -1.000000000000000000, -3.469446951953572774E-16, 0.000000000000000000 ) ) ;
#8398 = FACE_OUTER_BOUND ( 'NONE', #4556, .T. ) ;
#8399 = CARTESIAN_POINT ( 'NONE',  ( -61.13531646874998415, 12.39062499965860198, 1.500000000000002220 ) ) ;
#8400 = CARTESIAN_POINT ( 'NONE',  ( -62.86468353124998742, 16.03645833299193768, 1.999225269531025972 ) ) ;
#8401 = EDGE_CURVE ( 'NONE', #9681, #1845, #4755, .T. ) ;
#8402 = CARTESIAN_POINT ( 'NONE',  ( -61.99999999999998579, 12.56249999999999822, 0.5000000000000013323 ) ) ;
#8403 =( BOUNDED_CURVE ( )  B_SPLINE_CURVE ( 2, ( #1199, #2756, #7928, #7815, #5293, #1143, #8705, #8816, #2933 ),
 .UNSPECIFIED., .F., .T. ) 
 B_SPLINE_CURVE_WITH_KNOTS ( ( 3, 2, 2, 2, 3 ),
 ( 0.2578125000000000000, 0.2604166666666666852, 0.2656250000000000000, 0.2708333333333333148, 0.2734375000000000000 ),
 .UNSPECIFIED. ) 
 CURVE ( )  GEOMETRIC_REPRESENTATION_ITEM ( )  RATIONAL_B_SPLINE_CURVE ( ( 0.9330127018922194093, 0.9330127018922194093, 1.000000000000000000, 0.8660254037844387076, 1.000000000000000000, 0.8660254037844387076, 1.000000000000000000, 0.9330127018922194093, 0.9330127018922194093 ) ) 
 REPRESENTATION_ITEM ( '' )  );
#8404 = DIRECTION ( 'NONE',  ( 1.000000000000000000, 0.000000000000000000, 0.000000000000000000 ) ) ;
#8405 = CARTESIAN_POINT ( 'NONE',  ( -61.56765823437498852, 8.598958332991934128, 2.248837904296538515 ) ) ;
#8406 = DIRECTION ( 'NONE',  ( -1.000000000000000000, -0.000000000000000000, -0.000000000000000000 ) ) ;
#8407 = ORIENTED_EDGE ( 'NONE', *, *, #4985, .T. ) ;
#8408 = VECTOR ( 'NONE', #883, 1000.000000000000000 ) ;
#8409 = LINE ( 'NONE', #10539, #4231 ) ;
#8410 = DIRECTION ( 'NONE',  ( 0.000000000000000000, 0.000000000000000000, -1.000000000000000000 ) ) ;
#8411 = CARTESIAN_POINT ( 'NONE',  ( -62.86468353124999453, 14.70312499965860020, 1.500000000000002220 ) ) ;
#8412 = CARTESIAN_POINT ( 'NONE',  ( -62.43234176562499016, 11.74479166632526805, 2.248837904296538071 ) ) ;
#8413 = CARTESIAN_POINT ( 'NONE',  ( -61.99999999999999289, 15.07812499965860376, 2.498450539062049724 ) ) ;
#8414 = CARTESIAN_POINT ( 'NONE',  ( 190.0000000000000000, -6.123233995736783046E-16, 4.000000000000000000 ) ) ;
#8415 = EDGE_LOOP ( 'NONE', ( #5029, #9792, #3207, #10512 ) ) ;
#8416 = CARTESIAN_POINT ( 'NONE',  ( -60.99999999999998579, 14.00000000000000000, 1.500000000000002220 ) ) ;
#8417 = CARTESIAN_POINT ( 'NONE',  ( -61.56765823437498142, 8.932291666325268054, 0.7511620957034663704 ) ) ;
#8418 = CARTESIAN_POINT ( 'NONE',  ( -61.99999999999998579, 11.90624999931720396, 2.654700538379254571 ) ) ;
#8419 = ORIENTED_EDGE ( 'NONE', *, *, #9500, .F. ) ;
#8420 = EDGE_CURVE ( 'NONE', #10334, #3864, #5511, .T. ) ;
#8421 = CARTESIAN_POINT ( 'NONE',  ( -61.73205080756886076, 9.448664549684629321, 2.500000000000003109 ) ) ;
#8422 = CARTESIAN_POINT ( 'NONE',  ( -62.43234176562499016, 13.99479166632526805, 2.248837904296538071 ) ) ;
#8423 = FACE_OUTER_BOUND ( 'NONE', #2634, .T. ) ;
#8424 = EDGE_LOOP ( 'NONE', ( #4088, #6482, #6362, #6672 ) ) ;
#8425 = DIRECTION ( 'NONE',  ( -1.000000000000000000, 0.000000000000000000, 0.000000000000000000 ) ) ;
#8426 = CARTESIAN_POINT ( 'NONE',  ( -62.86468353124998742, 13.53645833299193413, 1.999225269531025972 ) ) ;
#8427 = FACE_OUTER_BOUND ( 'NONE', #8173, .T. ) ;
#8428 = DIRECTION ( 'NONE',  ( 0.000000000000000000, -5.421010862427519705E-17, 1.000000000000000000 ) ) ;
#8429 = ORIENTED_EDGE ( 'NONE', *, *, #811, .F. ) ;
#8430 = DIRECTION ( 'NONE',  ( 0.000000000000000000, 0.000000000000000000, -1.000000000000000000 ) ) ;
#8431 = ORIENTED_EDGE ( 'NONE', *, *, #1448, .T. ) ;
#8432 = CARTESIAN_POINT ( 'NONE',  ( -61.49999999999998579, 10.79166666666666607, 0.6339745962155628467 ) ) ;
#8433 = ORIENTED_EDGE ( 'NONE', *, *, #2745, .T. ) ;
#8434 = CARTESIAN_POINT ( 'NONE',  ( -62.86468353124998742, 9.536458332991935904, 1.999225269531025972 ) ) ;
#8435 = CARTESIAN_POINT ( 'NONE',  ( -105.0000000000000000, 2.500000000000000000, 4.000000000000000000 ) ) ;
#8436 = CARTESIAN_POINT ( 'NONE',  ( -61.99999999999998579, 13.07812499965860198, 2.498450539062049724 ) ) ;
#8437 = DIRECTION ( 'NONE',  ( -3.965082230804130220E-16, 1.000000000000000000, -0.000000000000000000 ) ) ;
#8438 = ORIENTED_EDGE ( 'NONE', *, *, #9482, .F. ) ;
#8439 = CARTESIAN_POINT ( 'NONE',  ( -44.00000000000000711, -14.00000000000000888, 3.999999999999999112 ) ) ;
#8440 = B_SPLINE_CURVE_WITH_KNOTS ( 'NONE', 3,
 ( #6176, #344, #7846, #6238, #9622, #8794 ),
 .UNSPECIFIED., .F., .F.,
 ( 4, 2, 4 ),
 ( 0.003549988921687060022, 0.003971677118101640293, 0.004393365314516220997 ),
 .UNSPECIFIED. ) ;
#8441 = ORIENTED_EDGE ( 'NONE', *, *, #2162, .F. ) ;
#8442 = DIRECTION ( 'NONE',  ( 0.000000000000000000, 1.084202172485504434E-16, -1.000000000000000000 ) ) ;
#8443 = ADVANCED_FACE ( 'NONE', ( #1334 ), #8942, .T. ) ;
#8444 = CARTESIAN_POINT ( 'NONE',  ( -62.86468353124998742, 15.22395833299193590, 1.999225269531025972 ) ) ;
#8445 = DIRECTION ( 'NONE',  ( -0.000000000000000000, -0.000000000000000000, 1.000000000000000000 ) ) ;
#8446 = DIRECTION ( 'NONE',  ( 0.000000000000000000, -1.000000000000000000, 0.000000000000000000 ) ) ;
#8447 = DIRECTION ( 'NONE',  ( -0.000000000000000000, -1.000000000000000000, -0.000000000000000000 ) ) ;
#8448 = CARTESIAN_POINT ( 'NONE',  ( -62.86468353124999453, 13.01562499965860198, 1.500000000000002220 ) ) ;
#8449 = CARTESIAN_POINT ( 'NONE',  ( -61.99999999999998579, 15.82812499965860020, 2.498450539062049724 ) ) ;
#8450 = CARTESIAN_POINT ( 'NONE',  ( -61.99999999999998579, 14.78124999931720218, 0.5000000000000013323 ) ) ;
#8451 = CARTESIAN_POINT ( 'NONE',  ( -61.49999999999998579, 13.51041666598387003, 0.6339745962155628467 ) ) ;
#8452 = CARTESIAN_POINT ( 'NONE',  ( -62.43234176562499016, 9.057291666325268054, 2.248837904296538071 ) ) ;
#8453 = CARTESIAN_POINT ( 'NONE',  ( -61.99999999999998579, 26.00000000000000355, 1.500000000000002220 ) ) ;
#8454 = VERTEX_POINT ( 'NONE', #8163 ) ;
#8455 = DIRECTION ( 'NONE',  ( 0.000000000000000000, 0.000000000000000000, 1.000000000000000000 ) ) ;
#8456 = CARTESIAN_POINT ( 'NONE',  ( -62.99999999999998579, 12.60416666666666607, 0.9226497308103756012 ) ) ;
#8457 = EDGE_CURVE ( 'NONE', #3127, #2471, #9396, .T. ) ;
#8458 = CARTESIAN_POINT ( 'NONE',  ( -62.43234176562498305, 14.91145833299193590, 0.7511620957034662593 ) ) ;
#8459 = CARTESIAN_POINT ( 'NONE',  ( -61.56765823437498852, 10.53645833299193413, 2.248837904296538515 ) ) ;
#8460 = CARTESIAN_POINT ( 'NONE',  ( -61.56765823437498852, 15.59895833299193590, 2.248837904296538515 ) ) ;
#8461 = CARTESIAN_POINT ( 'NONE',  ( -114.9999999999999289, -7.999999999999998224, -2.000000000000000000 ) ) ;
#8462 = ORIENTED_EDGE ( 'NONE', *, *, #9409, .F. ) ;
#8463 = CARTESIAN_POINT ( 'NONE',  ( -62.99999999999998579, 14.64583333333333393, 2.077350269189627952 ) ) ;
#8464 = CARTESIAN_POINT ( 'NONE',  ( -62.86468353124999453, 8.765624999658601979, 1.500000000000002220 ) ) ;
#8465 = MANIFOLD_SOLID_BREP ( 'M2 Clearance Hole1', #206 ) ;
#8466 = SURFACE_STYLE_FILL_AREA ( #8579 ) ;
#8467 = CARTESIAN_POINT ( 'NONE',  ( -62.99999999999998579, 12.82291666598386826, 0.9226497308103756012 ) ) ;
#8468 = VERTEX_POINT ( 'NONE', #5420 ) ;
#8469 = CARTESIAN_POINT ( 'NONE',  ( -61.99999999999998579, 16.00000000000000000, 1.500000000000002220 ) ) ;
#8470 = AXIS2_PLACEMENT_3D ( 'NONE', #2101, #1208, #4588 ) ;
#8471 = CARTESIAN_POINT ( 'NONE',  ( -62.43234176562498305, 12.16145833299193413, 0.7511620957034662593 ) ) ;
#8472 = EDGE_LOOP ( 'NONE', ( #142, #5588, #9517, #5920, #3508, #666, #8481, #4982 ) ) ;
#8473 = EDGE_CURVE ( 'NONE', #2680, #1405, #4033, .T. ) ;
#8474 = DIRECTION ( 'NONE',  ( -0.000000000000000000, -0.000000000000000000, -1.000000000000000000 ) ) ;
#8475 = CARTESIAN_POINT ( 'NONE',  ( -62.43234176562499016, 12.80729166632526805, 2.248837904296538071 ) ) ;
#8476 = CARTESIAN_POINT ( 'NONE',  ( -61.73205080756886076, 11.41741454900183328, 2.500000000000003109 ) ) ;
#8477=STYLED_ITEM('',(#11027),#8688);
#8478 = PRODUCT_DEFINITION ( 'UNKNOWN', '', #10277, #10921 ) ;
#8479 = ORIENTED_EDGE ( 'NONE', *, *, #2918, .F. ) ;
#8480 = CARTESIAN_POINT ( 'NONE',  ( -5.404070203482436163E-16, 0.2499999999999982792, 1.454823465665887605 ) ) ;
#8481 = ORIENTED_EDGE ( 'NONE', *, *, #2143, .T. ) ;
#8482 = FACE_OUTER_BOUND ( 'NONE', #9603, .T. ) ;
#8483 = AXIS2_PLACEMENT_3D ( 'NONE', #9174, #781, #8246 ) ;
#8484 = ORIENTED_EDGE ( 'NONE', *, *, #3094, .F. ) ;
#8485 = ORIENTED_EDGE ( 'NONE', *, *, #9509, .T. ) ;
#8486 = CIRCLE ( 'NONE', #3162, 2.500000000000002220 ) ;
#8487 = CARTESIAN_POINT ( 'NONE',  ( -62.86468353124998032, 9.244791666325268054, 1.000774730468978246 ) ) ;
#8488 = CARTESIAN_POINT ( 'NONE',  ( -61.49999999999998579, 14.20833333333333393, 2.366025403784441927 ) ) ;
#8489 = AXIS2_PLACEMENT_3D ( 'NONE', #5051, #60, #4165 ) ;
#8490 = CARTESIAN_POINT ( 'NONE',  ( -62.86468353124999453, 13.26562499965860198, 1.500000000000002220 ) ) ;
#8491 = LINE ( 'NONE', #7662, #5539 ) ;
#8492 = EDGE_LOOP ( 'NONE', ( #574, #10135, #7813, #9924 ) ) ;
#8493 = CYLINDRICAL_SURFACE ( 'NONE', #8887, 1.099999999999989875 ) ;
#8494 = AXIS2_PLACEMENT_3D ( 'NONE', #7565, #10844, #10588 ) ;
#8495 = VERTEX_POINT ( 'NONE', #8990 ) ;
#8496 = CARTESIAN_POINT ( 'NONE',  ( -61.73205080756886076, 12.69866454968462754, 2.500000000000003109 ) ) ;
#8497 = CARTESIAN_POINT ( 'NONE',  ( -62.43234176562498305, 14.66145833299193413, 0.7511620957034662593 ) ) ;
#8498 = VECTOR ( 'NONE', #6955, 1000.000000000000000 ) ;
#8499 = DIRECTION ( 'NONE',  ( 0.000000000000000000, 0.000000000000000000, -1.000000000000000000 ) ) ;
#8500 = CARTESIAN_POINT ( 'NONE',  ( -61.99999999999998579, 16.00000000000000000, 2.500000000000000444 ) ) ;
#8501 = EDGE_CURVE ( 'NONE', #2937, #8468, #10779, .T. ) ;
#8502 = CARTESIAN_POINT ( 'NONE',  ( -60.99999999999998579, 10.75000000000000000, 1.500000000000002220 ) ) ;
#8503 = CARTESIAN_POINT ( 'NONE',  ( -62.86468353124999453, 13.03645833299193413, 1.999225269531025750 ) ) ;
#8504 = CARTESIAN_POINT ( 'NONE',  ( -62.43234176562498305, 8.911458332991934128, 0.7511620957034662593 ) ) ;
#8505 = DIRECTION ( 'NONE',  ( -0.000000000000000000, -1.000000000000000000, -0.000000000000000000 ) ) ;
#8506 = CARTESIAN_POINT ( 'NONE',  ( -109.9999999999999289, 33.00000000000000711, -2.000000000000000000 ) ) ;
#8507 = CARTESIAN_POINT ( 'NONE',  ( -61.56765823437498142, 9.182291666325268054, 0.7511620957034663704 ) ) ;
#8508 = DIRECTION ( 'NONE',  ( 0.000000000000000000, 0.000000000000000000, -1.000000000000000000 ) ) ;
#8509 = VERTEX_POINT ( 'NONE', #1380 ) ;
#8510 = DIRECTION ( 'NONE',  ( 0.000000000000000000, 0.000000000000000000, 1.000000000000000000 ) ) ;
#8511 = EDGE_CURVE ( 'NONE', #4954, #6713, #380, .T. ) ;
#8512 = CARTESIAN_POINT ( 'NONE',  ( -79.09999999999998010, -11.50000000000000711, -2.000000000000001332 ) ) ;
#8513 = VECTOR ( 'NONE', #7774, 1000.000000000000000 ) ;
#8514 = CARTESIAN_POINT ( 'NONE',  ( -61.99999999999999289, 15.26562499965860020, 2.498450539062049724 ) ) ;
#8515 = CARTESIAN_POINT ( 'NONE',  ( -61.99999999999998579, 11.64062499965860198, 0.5015494609379544944 ) ) ;
#8516 = CARTESIAN_POINT ( 'NONE',  ( -62.43234176562499016, 15.55729166632526628, 2.248837904296538071 ) ) ;
#8517 = FILL_AREA_STYLE_COLOUR ( '', #2532 ) ;
#8518 = VERTEX_POINT ( 'NONE', #7271 ) ;
#8519 = CARTESIAN_POINT ( 'NONE',  ( -60.99999999999998579, 14.49999999999999822, 1.500000000000002220 ) ) ;
#8520 = CARTESIAN_POINT ( 'NONE',  ( -62.43234176562499016, 9.057291666325268054, 2.248837904296538071 ) ) ;
#8521 = MANIFOLD_SOLID_BREP ( 'AdvancedHole1', #2514 ) ;
#8522 =( NAMED_UNIT ( * ) SI_UNIT ( $, .STERADIAN. ) SOLID_ANGLE_UNIT ( ) );
#8523 = CARTESIAN_POINT ( 'NONE',  ( -62.49999999999998579, 13.55208333265053433, 0.6339745962155627357 ) ) ;
#8524 = CARTESIAN_POINT ( 'NONE',  ( -62.26794919243111082, 14.57366454968463110, 0.5000000000000013323 ) ) ;
#8525 = ORIENTED_EDGE ( 'NONE', *, *, #2143, .F. ) ;
#8526 = FACE_OUTER_BOUND ( 'NONE', #10697, .T. ) ;
#8527 = CARTESIAN_POINT ( 'NONE',  ( -61.99999999999999289, 11.51562499965860020, 2.498450539062049724 ) ) ;
#8528 = CARTESIAN_POINT ( 'NONE',  ( -61.99999999999998579, 8.000000000000000000, 0.5000000000000013323 ) ) ;
#8529 = CARTESIAN_POINT ( 'NONE',  ( -61.99999999999998579, 12.93750000000000000, 2.500000000000002665 ) ) ;
#8530 = ORIENTED_EDGE ( 'NONE', *, *, #4281, .T. ) ;
#8531 = EDGE_CURVE ( 'NONE', #1996, #3410, #4649, .T. ) ;
#8532 = CARTESIAN_POINT ( 'NONE',  ( -61.99999999999998579, 10.31250000000000000, 0.5000000000000013323 ) ) ;
#8533 = CARTESIAN_POINT ( 'NONE',  ( -62.43234176562499016, 12.55729166632526805, 2.248837904296538071 ) ) ;
#8534 = DIRECTION ( 'NONE',  ( 0.000000000000000000, 0.000000000000000000, -1.000000000000000000 ) ) ;
#8535 = CARTESIAN_POINT ( 'NONE',  ( -62.99999999999998579, 9.822916665983871809, 0.9226497308103756012 ) ) ;
#8536 = EDGE_CURVE ( 'NONE', #10601, #1452, #6605, .T. ) ;
#8537 = VERTEX_POINT ( 'NONE', #4140 ) ;
#8538 = DIRECTION ( 'NONE',  ( 0.000000000000000000, 0.000000000000000000, -1.000000000000000000 ) ) ;
#8539 = EDGE_LOOP ( 'NONE', ( #6252, #6762, #2976, #6153 ) ) ;
#8540 = CARTESIAN_POINT ( 'NONE',  ( -61.99999999999998579, 16.00000000000000000, 1.500000000000002220 ) ) ;
#8541 = CARTESIAN_POINT ( 'NONE',  ( -62.86468353124999453, 11.70312499965860198, 1.500000000000002220 ) ) ;
#8542 = ORIENTED_EDGE ( 'NONE', *, *, #3764, .F. ) ;
#8543 = CLOSED_SHELL ( 'NONE', ( #3333, #9518, #5594, #10780, #1308, #263, #2416, #8810, #5559, #868, #10818, #8766, #8709, #9541, #10507, #9146, #1973, #2262, #9379, #8614, #7945, #7556, #113, #1137, #10191, #1483, #1653, #10030, #6127, #7833, #10422, #5548, #5862, #316, #10129, #8371, #3829, #10527, #5634, #10125, #10717, #9725, #10759, #1272, #2622, #8666, #8013, #287, #10714, #5444, #3600, #1073, #2592, #10153, #180, #3724, #1830, #2567, #6148, #9547, #6644, #5775, #10081, #6374, #8046, #3213, #1708, #4137, #4796, #4615, #297, #3953, #538, #10229, #8796, #5584, #6202, #8951 ) ) ;
#8544 = CARTESIAN_POINT ( 'NONE',  ( -61.56765823437498142, 9.432291666325268054, 0.7511620957034663704 ) ) ;
#8545 = CARTESIAN_POINT ( 'NONE',  ( -61.13531646874998415, 13.41145833299193235, 1.000774730468978468 ) ) ;
#8546 = DIRECTION ( 'NONE',  ( -0.000000000000000000, -0.000000000000000000, -1.000000000000000000 ) ) ;
#8547 = ORIENTED_EDGE ( 'NONE', *, *, #1671, .F. ) ;
#8548 = AXIS2_PLACEMENT_3D ( 'NONE', #10795, #3184, #9967 ) ;
#8549 = DIRECTION ( 'NONE',  ( -1.000000000000000000, 0.000000000000000000, 0.000000000000000000 ) ) ;
#8550 = EDGE_CURVE ( 'NONE', #8575, #2384, #606, .T. ) ;
#8551 = VERTEX_POINT ( 'NONE', #9149 ) ;
#8552 = CARTESIAN_POINT ( 'NONE',  ( -62.26794919243111082, 10.82366454968462932, 0.5000000000000013323 ) ) ;
#8553 = CARTESIAN_POINT ( 'NONE',  ( -61.13531646874998415, 15.32812499965860020, 1.500000000000002220 ) ) ;
#8554 = CARTESIAN_POINT ( 'NONE',  ( -25.39999999999996305, 0.000000000000000000, 0.000000000000000000 ) ) ;
#8555 = LINE ( 'NONE', #5260, #6375 ) ;
#8556 =( BOUNDED_CURVE ( )  B_SPLINE_CURVE ( 2, ( #8068, #3603, #10379, #6337, #8661, #4432, #7832, #2775, #6162 ),
 .UNSPECIFIED., .F., .T. ) 
 B_SPLINE_CURVE_WITH_KNOTS ( ( 3, 2, 2, 2, 3 ),
 ( 0.5546875000000000000, 0.5572916666666666297, 0.5625000000000000000, 0.5677083333333333703, 0.5703125000000000000 ),
 .UNSPECIFIED. ) 
 CURVE ( )  GEOMETRIC_REPRESENTATION_ITEM ( )  RATIONAL_B_SPLINE_CURVE ( ( 0.9330127018922194093, 0.9330127018922194093, 1.000000000000000000, 0.8660254037844387076, 1.000000000000000000, 0.8660254037844387076, 1.000000000000000000, 0.9330127018922194093, 0.9330127018922194093 ) ) 
 REPRESENTATION_ITEM ( '' )  );
#8557 = CARTESIAN_POINT ( 'NONE',  ( -61.99999999999998579, 16.00000000000000000, 0.5000000000000041078 ) ) ;
#8558 = AXIS2_PLACEMENT_3D ( 'NONE', #8368, #25, #3352 ) ;
#8559 = CARTESIAN_POINT ( 'NONE',  ( -61.56765823437498852, 13.59895833299193413, 2.248837904296538515 ) ) ;
#8560 = AXIS2_PLACEMENT_3D ( 'NONE', #4405, #1920, #8763 ) ;
#8561 = CARTESIAN_POINT ( 'NONE',  ( -62.43234176562499016, 8.244791666325268054, 2.248837904296538071 ) ) ;
#8562 = FACE_OUTER_BOUND ( 'NONE', #9801, .T. ) ;
#8563 = DIRECTION ( 'NONE',  ( -0.000000000000000000, -1.000000000000000000, -0.000000000000000000 ) ) ;
#8564 = CARTESIAN_POINT ( 'NONE',  ( -61.13531646874998415, 9.119791666325268054, 1.999225269531026417 ) ) ;
#8565 = CARTESIAN_POINT ( 'NONE',  ( -31.99999999999997868, -14.00000000000000888, 3.999999999999999112 ) ) ;
#8566 = VERTEX_POINT ( 'NONE', #7380 ) ;
#8567 = CARTESIAN_POINT ( 'NONE',  ( -149.9999999999999716, 8.000000000000000000, 3.000000000000000000 ) ) ;
#8568 = DIRECTION ( 'NONE',  ( -0.000000000000000000, 1.000000000000000000, -0.000000000000000000 ) ) ;
#8569 = ADVANCED_FACE ( 'NONE', ( #756 ), #7418, .T. ) ;
#8570 = AXIS2_PLACEMENT_3D ( 'NONE', #7364, #8201, #9029 ) ;
#8571 = CARTESIAN_POINT ( 'NONE',  ( -62.43234176562499016, 15.74479166632526628, 2.248837904296538071 ) ) ;
#8572 = CARTESIAN_POINT ( 'NONE',  ( -61.13531646874998415, 10.84895833299193590, 1.000774730468978468 ) ) ;
#8573 = CARTESIAN_POINT ( 'NONE',  ( -61.56765823437498852, 9.286458332991935904, 2.248837904296538515 ) ) ;
#8574 = CARTESIAN_POINT ( 'NONE',  ( -62.49999999999998579, 13.13541666598387003, 2.366025403784441483 ) ) ;
#8575 = VERTEX_POINT ( 'NONE', #5024 ) ;
#8576 = CARTESIAN_POINT ( 'NONE',  ( -62.99999999999998579, 15.10416666666666785, 0.9226497308103756012 ) ) ;
#8577 = EDGE_CURVE ( 'NONE', #9081, #10876, #7433, .T. ) ;
#8578 = CARTESIAN_POINT ( 'NONE',  ( -61.56765823437498142, 8.432291666325268054, 0.7511620957034663704 ) ) ;
#8579 = FILL_AREA_STYLE ('',( #6130 ) ) ;
#8580 = VECTOR ( 'NONE', #3955, 1000.000000000000000 ) ;
#8581 = CARTESIAN_POINT ( 'NONE',  ( -61.99999999999998579, 12.78124999931720218, 0.3452994616207497591 ) ) ;
#8582 = CARTESIAN_POINT ( 'NONE',  ( -62.99999999999998579, 14.60416666666666430, 0.9226497308103756012 ) ) ;
#8583 = ORIENTED_EDGE ( 'NONE', *, *, #7295, .F. ) ;
#8584 = LINE ( 'NONE', #2805, #410 ) ;
#8585 = CARTESIAN_POINT ( 'NONE',  ( -61.99999999999999289, 11.14062499965860020, 0.5015494609379544944 ) ) ;
#8586 = LINE ( 'NONE', #2529, #10604 ) ;
#8587 = CARTESIAN_POINT ( 'NONE',  ( -61.99999999999998579, 11.03124999931720218, 0.5000000000000013323 ) ) ;
#8588 = ORIENTED_EDGE ( 'NONE', *, *, #4109, .F. ) ;
#8589 = CARTESIAN_POINT ( 'NONE',  ( -77.99999999999998579, 11.49999999999999645, -2.000000000000000000 ) ) ;
#8590 = CARTESIAN_POINT ( 'NONE',  ( -61.13531646874998415, 12.64062499965860198, 1.500000000000002220 ) ) ;
#8591 = CARTESIAN_POINT ( 'NONE',  ( -61.99999999999998579, 13.81249999999999822, 0.5000000000000013323 ) ) ;
#8592 = CARTESIAN_POINT ( 'NONE',  ( -62.99999999999998579, 9.572916665983870033, 0.9226497308103756012 ) ) ;
#8593 = ORIENTED_EDGE ( 'NONE', *, *, #4725, .F. ) ;
#8594 = CARTESIAN_POINT ( 'NONE',  ( -61.99999999999998579, 9.687500000000000000, 2.500000000000002665 ) ) ;
#8595 = ORIENTED_EDGE ( 'NONE', *, *, #6443, .T. ) ;
#8596 = CARTESIAN_POINT ( 'NONE',  ( -60.99999999999998579, 14.75000000000000000, 1.500000000000002220 ) ) ;
#8597 = CARTESIAN_POINT ( 'NONE',  ( -61.99999999999998579, 11.14062499965860020, 0.5015494609379544944 ) ) ;
#8598 = ADVANCED_FACE ( 'NONE', ( #8423 ), #9203, .T. ) ;
#8599 = ORIENTED_EDGE ( 'NONE', *, *, #5434, .T. ) ;
#8600 = CARTESIAN_POINT ( 'NONE',  ( -62.86468353124998742, 9.286458332991934128, 1.999225269531025972 ) ) ;
#8601 = CARTESIAN_POINT ( 'NONE',  ( -62.99999999999998579, 13.86458333265053611, 2.077350269189627952 ) ) ;
#8602 = CARTESIAN_POINT ( 'NONE',  ( -61.56765823437498852, 13.59895833299193413, 2.248837904296538515 ) ) ;
#8603 = CARTESIAN_POINT ( 'NONE',  ( -61.99999999999998579, 9.281249999317203958, 0.5000000000000013323 ) ) ;
#8604 = ORIENTED_EDGE ( 'NONE', *, *, #4867, .T. ) ;
#8605 = DIRECTION ( 'NONE',  ( -0.000000000000000000, -0.000000000000000000, 1.000000000000000000 ) ) ;
#8606 = MANIFOLD_SOLID_BREP ( 'AdvancedHole1', #1093 ) ;
#8607 = ORIENTED_EDGE ( 'NONE', *, *, #2457, .T. ) ;
#8608 = CARTESIAN_POINT ( 'NONE',  ( -61.99999999999998579, 16.00000000000000000, 1.500000000000002220 ) ) ;
#8609 = CARTESIAN_POINT ( 'NONE',  ( -61.13531646874998415, 15.07812499965860020, 1.500000000000002220 ) ) ;
#8610 = CARTESIAN_POINT ( 'NONE',  ( -62.99999999999998579, 8.843749999317203958, 1.500000000000001998 ) ) ;
#8611 = CARTESIAN_POINT ( 'NONE',  ( -61.99999999999998579, 12.43749999999999822, 2.500000000000002665 ) ) ;
#8612 = CARTESIAN_POINT ( 'NONE',  ( -61.99999999999998579, 16.00000000000000000, 2.500000000000000444 ) ) ;
#8613 = CARTESIAN_POINT ( 'NONE',  ( -62.86468353124999453, 13.53645833299193413, 1.999225269531025750 ) ) ;
#8614 = ADVANCED_FACE ( 'NONE', ( #10811 ), #7432, .T. ) ;
#8615 = CARTESIAN_POINT ( 'NONE',  ( -61.56765823437498142, 8.369791666325268054, 0.7511620957034663704 ) ) ;
#8616 = CARTESIAN_POINT ( 'NONE',  ( -49.99998799999998766, -14.00000000000001243, 3.141811147483251965 ) ) ;
#8617 = CARTESIAN_POINT ( 'NONE',  ( 0.5000000000000000000, 0.2499999999999998335, 1.911797424705720116 ) ) ;
#8618 = CARTESIAN_POINT ( 'NONE',  ( -61.13531646874998415, 9.640624999658601979, 1.500000000000002220 ) ) ;
#8619 = CARTESIAN_POINT ( 'NONE',  ( -61.99999999999998579, 16.00000000000000000, 0.5000000000000041078 ) ) ;
#8620 = ORIENTED_EDGE ( 'NONE', *, *, #3305, .F. ) ;
#8621 = CARTESIAN_POINT ( 'NONE',  ( -49.99999999999998579, -15.00000000000001243, 83.15773105863907233 ) ) ;
#8622 = CARTESIAN_POINT ( 'NONE',  ( -60.99999999999998579, 11.23958333265053611, 0.9226497308103762673 ) ) ;
#8623 =( BOUNDED_CURVE ( )  B_SPLINE_CURVE ( 2, ( #884, #1721, #1047, #10323, #6892, #4263, #54, #3438, #2607 ),
 .UNSPECIFIED., .F., .T. ) 
 B_SPLINE_CURVE_WITH_KNOTS ( ( 3, 2, 2, 2, 3 ),
 ( 0.5234375000000000000, 0.5260416666666666297, 0.5312500000000000000, 0.5364583333333333703, 0.5390625000000000000 ),
 .UNSPECIFIED. ) 
 CURVE ( )  GEOMETRIC_REPRESENTATION_ITEM ( )  RATIONAL_B_SPLINE_CURVE ( ( 0.9330127018922194093, 0.9330127018922194093, 1.000000000000000000, 0.8660254037844387076, 1.000000000000000000, 0.8660254037844387076, 1.000000000000000000, 0.9330127018922194093, 0.9330127018922194093 ) ) 
 REPRESENTATION_ITEM ( '' )  );
#8624 = CARTESIAN_POINT ( 'NONE',  ( -62.86468353124999453, 15.97395833299193590, 1.999225269531025750 ) ) ;
#8625 = CARTESIAN_POINT ( 'NONE',  ( -61.56765823437498142, 10.61979166632526805, 0.7511620957034663704 ) ) ;
#8626 = CARTESIAN_POINT ( 'NONE',  ( -61.56765823437498142, 8.869791666325268054, 0.7511620957034663704 ) ) ;
#8627 = SURFACE_SIDE_STYLE ('',( #5165 ) ) ;
#8628 = ORIENTED_EDGE ( 'NONE', *, *, #4352, .T. ) ;
#8629 = CARTESIAN_POINT ( 'NONE',  ( -62.49999999999998579, 14.66666666666666607, 2.366025403784441483 ) ) ;
#8630 = CARTESIAN_POINT ( 'NONE',  ( -61.99999999999999289, 10.45312499965860198, 0.5015494609379544944 ) ) ;
#8631 = PRESENTATION_STYLE_ASSIGNMENT (( #1743 ) ) ;
#8632 = CARTESIAN_POINT ( 'NONE',  ( -62.49999999999998579, 12.80208333265053611, 0.6339745962155627357 ) ) ;
#8633 = CARTESIAN_POINT ( 'NONE',  ( -62.26794919243111082, 13.07366454968462932, 0.5000000000000013323 ) ) ;
#8634 = ORIENTED_EDGE ( 'NONE', *, *, #1204, .T. ) ;
#8635 = DIRECTION ( 'NONE',  ( 0.000000000000000000, 0.000000000000000000, -1.000000000000000000 ) ) ;
#8636 = CARTESIAN_POINT ( 'NONE',  ( -61.13531646874997705, 12.05729166632526628, 1.999225269531026417 ) ) ;
#8637 = CARTESIAN_POINT ( 'NONE',  ( -62.99999999999998579, 15.60416666666666607, 0.9226497308103756012 ) ) ;
#8638 = CARTESIAN_POINT ( 'NONE',  ( -61.99999999999998579, 15.43749999999999822, 2.500000000000002665 ) ) ;
#8639 = ORIENTED_EDGE ( 'NONE', *, *, #8252, .T. ) ;
#8640 = CARTESIAN_POINT ( 'NONE',  ( -62.99999999999998579, 11.12500000000000000, 1.500000000000001998 ) ) ;
#8641 = DIRECTION ( 'NONE',  ( -0.000000000000000000, -1.000000000000000000, -0.000000000000000000 ) ) ;
#8642 = CARTESIAN_POINT ( 'NONE',  ( -62.86468353124999453, 13.76562499965860198, 1.500000000000002220 ) ) ;
#8643 = CARTESIAN_POINT ( 'NONE',  ( -60.99999999999998579, 10.25000000000000000, 1.500000000000002220 ) ) ;
#8644 = CARTESIAN_POINT ( 'NONE',  ( -60.99999999999998579, 9.718749999317202182, 1.500000000000002220 ) ) ;
#8645 = ORIENTED_EDGE ( 'NONE', *, *, #7274, .F. ) ;
#8646 = MECHANICAL_DESIGN_GEOMETRIC_PRESENTATION_REPRESENTATION (  '', ( #6538 ), #1206 ) ;
#8647 = CARTESIAN_POINT ( 'NONE',  ( 145.0000000000000284, 5.500000000000000000, 3.000000000000000888 ) ) ;
#8648 = CARTESIAN_POINT ( 'NONE',  ( -61.99999999999998579, 14.99999999999998579, 1.500000000000002220 ) ) ;
#8649 = EDGE_CURVE ( 'NONE', #10734, #9779, #9704, .T. ) ;
#8650 = CARTESIAN_POINT ( 'NONE',  ( -61.56765823437498852, 10.78645833299193413, 2.248837904296538515 ) ) ;
#8651 = ORIENTED_EDGE ( 'NONE', *, *, #8322, .F. ) ;
#8652 = CARTESIAN_POINT ( 'NONE',  ( -62.43234176562498305, 9.223958332991935904, 0.7511620957034662593 ) ) ;
#8653 = DIRECTION ( 'NONE',  ( -0.000000000000000000, -1.000000000000000000, -0.000000000000000000 ) ) ;
#8654 = CARTESIAN_POINT ( 'NONE',  ( -62.43234176562498305, 14.22395833299193413, 0.7511620957034662593 ) ) ;
#8655 = CARTESIAN_POINT ( 'NONE',  ( -61.99999999999998579, 13.18750000000000000, 2.500000000000002665 ) ) ;
#8656 = ORIENTED_EDGE ( 'NONE', *, *, #2073, .F. ) ;
#8657 = CARTESIAN_POINT ( 'NONE',  ( -62.26794919243111082, 9.426335450315370679, 2.500000000000003109 ) ) ;
#8658 = CIRCLE ( 'NONE', #327, 6.000000000000005329 ) ;
#8659 = CIRCLE ( 'NONE', #7963, 0.9999999999999983347 ) ;
#8660 = ORIENTED_EDGE ( 'NONE', *, *, #3636, .F. ) ;
#8661 = CARTESIAN_POINT ( 'NONE',  ( -60.99999999999998579, 12.71874999931720396, 1.500000000000002220 ) ) ;
#8662 = CARTESIAN_POINT ( 'NONE',  ( -62.99999999999998579, 8.375000000000000000, 1.500000000000001998 ) ) ;
#8663 = CYLINDRICAL_SURFACE ( 'NONE', #3254, 1.000000000000000000 ) ;
#8664 = CARTESIAN_POINT ( 'NONE',  ( -61.99999999999998579, 14.99999999999998579, 1.500000000000002220 ) ) ;
#8665 = DIRECTION ( 'NONE',  ( -1.000000000000000000, -2.478176394252581696E-17, 0.000000000000000000 ) ) ;
#8666 = ADVANCED_FACE ( 'NONE', ( #5918 ), #1750, .T. ) ;
#8667 = CARTESIAN_POINT ( 'NONE',  ( -61.13531646874997705, 14.36979166632527161, 1.999225269531026417 ) ) ;
#8668 = CIRCLE ( 'NONE', #8489, 1.000000000000000000 ) ;
#8669 = CARTESIAN_POINT ( 'NONE',  ( -62.43234176562499016, 8.994791666325268054, 2.248837904296538071 ) ) ;
#8670 = CARTESIAN_POINT ( 'NONE',  ( -61.99999999999998579, 9.312500000000000000, 0.5000000000000013323 ) ) ;
#8671 = CARTESIAN_POINT ( 'NONE',  ( 1.299999999999999600, 1.000000000000000000, 0.000000000000000000 ) ) ;
#8672 = CARTESIAN_POINT ( 'NONE',  ( -62.86468353124998742, 10.28645833299193590, 1.999225269531025972 ) ) ;
#8673 = ADVANCED_FACE ( 'NONE', ( #9522 ), #1017, .F. ) ;
#8674 = VECTOR ( 'NONE', #5531, 1000.000000000000000 ) ;
#8675 = DIRECTION ( 'NONE',  ( -1.000000000000000000, 0.000000000000000000, -0.000000000000000000 ) ) ;
#8676 = ORIENTED_EDGE ( 'NONE', *, *, #2088, .T. ) ;
#8677 = CARTESIAN_POINT ( 'NONE',  ( 0.5999999999999999778, 1.636698849489768475E-16, -1.336466033005844434 ) ) ;
#8678 = CYLINDRICAL_SURFACE ( 'NONE', #758, 0.9999999999999981126 ) ;
#8679 = EDGE_CURVE ( 'NONE', #2164, #5869, #10789, .T. ) ;
#8680 = VECTOR ( 'NONE', #5868, 1000.000000000000000 ) ;
#8681 = CARTESIAN_POINT ( 'NONE',  ( -62.86468353124998032, 14.93229166632526983, 1.000774730468978024 ) ) ;
#8682 = CARTESIAN_POINT ( 'NONE',  ( -61.56765823437498852, 12.28645833299193413, 2.248837904296538515 ) ) ;
#8683 = CARTESIAN_POINT ( 'NONE',  ( -61.56765823437498142, 8.369791666325268054, 0.7511620957034663704 ) ) ;
#8684 = SURFACE_STYLE_USAGE ( .BOTH. , #8627 ) ;
#8685 = VERTEX_POINT ( 'NONE', #8528 ) ;
#8686 = CARTESIAN_POINT ( 'NONE',  ( -62.99999999999998579, 15.62500000000000000, 1.500000000000001998 ) ) ;
#8687 = CARTESIAN_POINT ( 'NONE',  ( -62.43234176562498305, 10.47395833299193413, 0.7511620957034662593 ) ) ;
#8688 = MANIFOLD_SOLID_BREP ( 'Thread1', #8543 ) ;
#8689 = DIRECTION ( 'NONE',  ( 0.000000000000000000, 0.000000000000000000, 1.000000000000000000 ) ) ;
#8690 = CARTESIAN_POINT ( 'NONE',  ( -61.13531646874998415, 15.80729166632526628, 1.999225269531026417 ) ) ;
#8691 = AXIS2_PLACEMENT_3D ( 'NONE', #387, #3713, #449 ) ;
#8692 = CARTESIAN_POINT ( 'NONE',  ( -61.99999999999998579, 14.03124999931720218, 0.3452994616207497591 ) ) ;
#8693 = DIRECTION ( 'NONE',  ( -0.000000000000000000, -0.000000000000000000, 1.000000000000000000 ) ) ;
#8694 = VERTEX_POINT ( 'NONE', #4236 ) ;
#8695 = CYLINDRICAL_SURFACE ( 'NONE', #599, 1.000000000000000888 ) ;
#8696 = AXIS2_PLACEMENT_3D ( 'NONE', #9860, #9633, #5398 ) ;
#8697 =( BOUNDED_CURVE ( )  B_SPLINE_CURVE ( 2, ( #2303, #5687, #636, #9240, #1681, #4953, #6738, #8354, #684 ),
 .UNSPECIFIED., .F., .F. ) 
 B_SPLINE_CURVE_WITH_KNOTS ( ( 3, 2, 2, 2, 3 ),
 ( 0.2890624999999999445, 0.2916666666666666852, 0.2968750000000000000, 0.3020833333333333148, 0.3046875000000000000 ),
 .UNSPECIFIED. ) 
 CURVE ( )  GEOMETRIC_REPRESENTATION_ITEM ( )  RATIONAL_B_SPLINE_CURVE ( ( 0.9330127018922192983, 0.9330127018922178550, 1.000000000000000000, 0.8660254037844387076, 1.000000000000000000, 0.8660254037844387076, 1.000000000000000000, 0.9330127018922194093, 0.9330127018922194093 ) ) 
 REPRESENTATION_ITEM ( '' )  );
#8698 = EDGE_CURVE ( 'NONE', #8768, #9263, #8586, .T. ) ;
#8699 = CARTESIAN_POINT ( 'NONE',  ( -61.13531646874997705, 11.30729166632526805, 1.999225269531026417 ) ) ;
#8700 = CARTESIAN_POINT ( 'NONE',  ( -61.99999999999998579, 8.890624999658601979, 0.5015494609379544944 ) ) ;
#8701 = AXIS2_PLACEMENT_3D ( 'NONE', #3003, #4095, #7490 ) ;
#8702 = CARTESIAN_POINT ( 'NONE',  ( -61.49999999999998579, 12.95833333333333215, 2.366025403784441927 ) ) ;
#8703 = ORIENTED_EDGE ( 'NONE', *, *, #9098, .F. ) ;
#8704 = CARTESIAN_POINT ( 'NONE',  ( -62.99999999999998579, 10.62499999999999822, 1.500000000000001998 ) ) ;
#8705 = CARTESIAN_POINT ( 'NONE',  ( -62.49999999999998579, 10.16666666666666785, 2.366025403784441483 ) ) ;
#8706 = CARTESIAN_POINT ( 'NONE',  ( -62.86468353124998032, 14.24479166632526983, 1.000774730468978246 ) ) ;
#8707 = CARTESIAN_POINT ( 'NONE',  ( -61.49999999999998579, 11.04166666666666607, 0.6339745962155628467 ) ) ;
#8708 = CARTESIAN_POINT ( 'NONE',  ( -62.99999999999998579, 9.864583332650536107, 2.077350269189627952 ) ) ;
#8709 = ADVANCED_FACE ( 'NONE', ( #4341 ), #6976, .T. ) ;
#8710 = ORIENTED_EDGE ( 'NONE', *, *, #8550, .F. ) ;
#8711 = LINE ( 'NONE', #3530, #7095 ) ;
#8712 = LINE ( 'NONE', #1030, #9010 ) ;
#8713 = ADVANCED_FACE ( 'NONE', ( #10354 ), #5233, .F. ) ;
#8714 = CARTESIAN_POINT ( 'NONE',  ( -61.13531646874998415, 10.80729166632526628, 1.999225269531026417 ) ) ;
#8715 = ORIENTED_EDGE ( 'NONE', *, *, #9509, .F. ) ;
#8716 = CARTESIAN_POINT ( 'NONE',  ( -62.86468353124998742, 10.53645833299193413, 1.999225269531025972 ) ) ;
#8717 = CARTESIAN_POINT ( 'NONE',  ( -61.99999999999998579, 16.00000000000000000, 1.500000000000002220 ) ) ;
#8718 = EDGE_CURVE ( 'NONE', #2286, #5975, #5289, .T. ) ;
#8719 = CARTESIAN_POINT ( 'NONE',  ( -62.86468353124999453, 14.01562499965860198, 1.500000000000002220 ) ) ;
#8720 = DIRECTION ( 'NONE',  ( 0.000000000000000000, 5.421010862427519705E-17, -1.000000000000000000 ) ) ;
#8721 = ORIENTED_EDGE ( 'NONE', *, *, #7522, .T. ) ;
#8722 = DIRECTION ( 'NONE',  ( -1.000000000000000000, -0.000000000000000000, -0.000000000000000000 ) ) ;
#8723 = VECTOR ( 'NONE', #9298, 999.9999999999998863 ) ;
#8724 = ORIENTED_EDGE ( 'NONE', *, *, #10949, .F. ) ;
#8725 = CARTESIAN_POINT ( 'NONE',  ( -61.99999999999998579, 15.15624999931720218, 2.500000000000002665 ) ) ;
#8726 = CARTESIAN_POINT ( 'NONE',  ( -62.99999999999998579, 8.354166666666666075, 0.9226497308103756012 ) ) ;
#8727 = CARTESIAN_POINT ( 'NONE',  ( -62.49999999999998579, 8.802083332650536107, 0.6339745962155627357 ) ) ;
#8728 = CYLINDRICAL_SURFACE ( 'NONE', #8150, 1.099999999999989875 ) ;
#8729 = CARTESIAN_POINT ( 'NONE',  ( -61.13531646874998415, 13.89062499965860198, 1.500000000000002220 ) ) ;
#8730 = CARTESIAN_POINT ( 'NONE',  ( -62.86468353124998032, 8.682291666325268054, 1.000774730468978246 ) ) ;
#8731 = CARTESIAN_POINT ( 'NONE',  ( -61.99999999999998579, 11.90624999931720041, 2.500000000000002665 ) ) ;
#8732 = FACE_BOUND ( 'NONE', #8128, .T. ) ;
#8733 = AXIS2_PLACEMENT_3D ( 'NONE', #10900, #4067, #3336 ) ;
#8734 = CARTESIAN_POINT ( 'NONE',  ( -62.43234176562498305, 10.72395833299193413, 0.7511620957034662593 ) ) ;
#8735 = CARTESIAN_POINT ( 'NONE',  ( 150.0000000000000000, 2.500000000000000444, 6.000000000000000000 ) ) ;
#8736 = ORIENTED_EDGE ( 'NONE', *, *, #901, .T. ) ;
#8737 = CARTESIAN_POINT ( 'NONE',  ( -61.49999999999998579, 13.92708333265053611, 2.366025403784441927 ) ) ;
#8738 = LINE ( 'NONE', #5107, #2707 ) ;
#8739 = ADVANCED_FACE ( 'NONE', ( #6861 ), #3355, .F. ) ;
#8740 = PRESENTATION_LAYER_ASSIGNMENT (  '', '', ( #2525 ) ) ;
#8741 = CARTESIAN_POINT ( 'NONE',  ( -61.99999999999998579, 10.03124999931720218, 0.5000000000000013323 ) ) ;
#8742 = CARTESIAN_POINT ( 'NONE',  ( -61.99999999999998579, 12.64062499965860198, 0.5015494609379544944 ) ) ;
#8743 = CONICAL_SURFACE ( 'NONE', #3949, 5.000000000000018652, 0.7853981633974430610 ) ;
#8744 = EDGE_CURVE ( 'NONE', #544, #7749, #2639, .T. ) ;
#8745 = CARTESIAN_POINT ( 'NONE',  ( -61.13531646874997705, 8.307291666325268054, 1.999225269531026417 ) ) ;
#8746 = VERTEX_POINT ( 'NONE', #9644 ) ;
#8747 = CARTESIAN_POINT ( 'NONE',  ( -62.49999999999998579, 15.83333333333333037, 0.6339745962155627357 ) ) ;
#8748 = CARTESIAN_POINT ( 'NONE',  ( -61.99999999999999289, 9.703124999658601979, 0.5015494609379544944 ) ) ;
#8749 = PRODUCT_CONTEXT ( 'NONE', #10086, 'mechanical' ) ;
#8750 = CARTESIAN_POINT ( 'NONE',  ( -62.43234176562498305, 15.16145833299193590, 0.7511620957034662593 ) ) ;
#8751 = CARTESIAN_POINT ( 'NONE',  ( -60.99999999999998579, 13.96874999931720218, 1.500000000000002220 ) ) ;
#8752 = DIRECTION ( 'NONE',  ( 1.000000000000000000, 0.000000000000000000, 0.000000000000000000 ) ) ;
#8753 = ORIENTED_EDGE ( 'NONE', *, *, #10813, .F. ) ;
#8754 = CIRCLE ( 'NONE', #5359, 23.99999999999999289 ) ;
#8755=STYLED_ITEM('',(#11027),#4773);
#8756 = FACE_OUTER_BOUND ( 'NONE', #9537, .T. ) ;
#8757 = CARTESIAN_POINT ( 'NONE',  ( -61.13531646874997705, 12.59895833299193590, 1.000774730468978468 ) ) ;
#8758 = CARTESIAN_POINT ( 'NONE',  ( -61.13531646874998415, 8.848958332991935904, 1.000774730468978468 ) ) ;
#8759 = CARTESIAN_POINT ( 'NONE',  ( -61.99999999999998579, 13.06250000000000178, 0.5000000000000013323 ) ) ;
#8760 = ORIENTED_EDGE ( 'NONE', *, *, #3189, .F. ) ;
#8761 = CARTESIAN_POINT ( 'NONE',  ( -61.99999999999998579, 12.43750000000000000, 2.654700538379254571 ) ) ;
#8762 = VECTOR ( 'NONE', #10350, 1000.000000000000000 ) ;
#8763 = DIRECTION ( 'NONE',  ( 0.000000000000000000, 0.000000000000000000, -1.000000000000000000 ) ) ;
#8764 = CARTESIAN_POINT ( 'NONE',  ( -61.13531646874998415, 14.66145833299193590, 1.000774730468978468 ) ) ;
#8765 = DIRECTION ( 'NONE',  ( -1.000000000000000000, 0.000000000000000000, -0.000000000000000000 ) ) ;
#8766 = ADVANCED_FACE ( 'NONE', ( #482 ), #249, .T. ) ;
#8767 = CARTESIAN_POINT ( 'NONE',  ( -60.99999999999998579, 10.46874999931720218, 1.500000000000002220 ) ) ;
#8768 = VERTEX_POINT ( 'NONE', #2090 ) ;
#8769 =( BOUNDED_CURVE ( )  B_SPLINE_CURVE ( 2, ( #6730, #7509, #1720, #4111, #9124, #2554, #7403, #10981, #2389 ),
 .UNSPECIFIED., .F., .T. ) 
 B_SPLINE_CURVE_WITH_KNOTS ( ( 3, 2, 2, 2, 3 ),
 ( 0.7109375000000000000, 0.7135416666666666297, 0.7187500000000000000, 0.7239583333333333703, 0.7265625000000000000 ),
 .UNSPECIFIED. ) 
 CURVE ( )  GEOMETRIC_REPRESENTATION_ITEM ( )  RATIONAL_B_SPLINE_CURVE ( ( 0.9330127018922194093, 0.9330127018922194093, 1.000000000000000000, 0.8660254037844387076, 1.000000000000000000, 0.8660254037844387076, 1.000000000000000000, 0.9330127018922194093, 0.9330127018922194093 ) ) 
 REPRESENTATION_ITEM ( '' )  );
#8770 = DIRECTION ( 'NONE',  ( -0.000000000000000000, -0.000000000000000000, 1.000000000000000000 ) ) ;
#8771 = FACE_OUTER_BOUND ( 'NONE', #7018, .T. ) ;
#8772 = CARTESIAN_POINT ( 'NONE',  ( -61.99999999999998579, 11.39062499965859843, 0.5015494609379544944 ) ) ;
#8773 = CARTESIAN_POINT ( 'NONE',  ( 0.2307700686259116507, -0.2500000000000000000, 1.812750528907549175 ) ) ;
#8774 = ORIENTED_EDGE ( 'NONE', *, *, #2647, .F. ) ;
#8775 = CARTESIAN_POINT ( 'NONE',  ( -61.99999999999998579, 10.70312499965860198, 0.5015494609379544944 ) ) ;
#8776 = CARTESIAN_POINT ( 'NONE',  ( -61.99999999999998579, 16.00000000000000000, -1.000000000000000000 ) ) ;
#8777 = CARTESIAN_POINT ( 'NONE',  ( -62.43234176562498305, 14.72395833299193413, 0.7511620957034662593 ) ) ;
#8778 = CARTESIAN_POINT ( 'NONE',  ( -61.73205080756886076, 8.917414549001833279, 2.500000000000003109 ) ) ;
#8779 = ORIENTED_EDGE ( 'NONE', *, *, #7365, .T. ) ;
#8780 = CARTESIAN_POINT ( 'NONE',  ( -60.99999999999998579, 10.52083333333333393, 0.9226497308103762673 ) ) ;
#8781 = VERTEX_POINT ( 'NONE', #8812 ) ;
#8782 = DIRECTION ( 'NONE',  ( 0.000000000000000000, -0.000000000000000000, 1.000000000000000000 ) ) ;
#8783 = CARTESIAN_POINT ( 'NONE',  ( -62.49999999999998579, 8.583333333333333925, 0.6339745962155627357 ) ) ;
#8784 = DIRECTION ( 'NONE',  ( 1.000000000000000000, 0.000000000000000000, 0.000000000000000000 ) ) ;
#8785 = DIRECTION ( 'NONE',  ( 1.000000000000000000, 0.000000000000000000, 0.000000000000000000 ) ) ;
#8786 = CARTESIAN_POINT ( 'NONE',  ( -61.13531646874998415, 16.07812499965860198, 1.500000000000002220 ) ) ;
#8787 = CARTESIAN_POINT ( 'NONE',  ( -62.43234176562499016, 14.55729166632526983, 2.248837904296538071 ) ) ;
#8788 = CARTESIAN_POINT ( 'NONE',  ( -62.86468353124998032, 10.18229166632526805, 1.000774730468978246 ) ) ;
#8789 = DIRECTION ( 'NONE',  ( 1.110223024625156540E-15, -1.000000000000000000, -0.000000000000000000 ) ) ;
#8790 = DIRECTION ( 'NONE',  ( -1.000000000000000000, 0.000000000000000000, -0.000000000000000000 ) ) ;
#8791 = CARTESIAN_POINT ( 'NONE',  ( -61.56765823437498142, 10.93229166632526805, 0.7511620957034663704 ) ) ;
#8792 = CARTESIAN_POINT ( 'NONE',  ( -61.13531646874998415, 16.14062499965860198, 1.500000000000002220 ) ) ;
#8793 = ORIENTED_EDGE ( 'NONE', *, *, #4021, .F. ) ;
#8794 = CARTESIAN_POINT ( 'NONE',  ( 0.000000000000000000, -0.2499999999999997780, -1.312875263449798879 ) ) ;
#8795 = DIRECTION ( 'NONE',  ( -0.000000000000000000, -1.000000000000000000, -0.000000000000000000 ) ) ;
#8796 = ADVANCED_FACE ( 'NONE', ( #2929 ), #10829, .T. ) ;
#8797 = VERTEX_POINT ( 'NONE', #1965 ) ;
#8798 = LINE ( 'NONE', #7131, #4997 ) ;
#8799 = CARTESIAN_POINT ( 'NONE',  ( -62.43234176562499016, 12.49479166632526805, 2.248837904296538071 ) ) ;
#8800 = CARTESIAN_POINT ( 'NONE',  ( -61.13531646874997705, 9.307291666325268054, 1.999225269531026417 ) ) ;
#8801 = CARTESIAN_POINT ( 'NONE',  ( 140.0000000000000284, -8.000000000000000000, 6.000000000000000000 ) ) ;
#8802 = ORIENTED_EDGE ( 'NONE', *, *, #6767, .F. ) ;
#8803 = CARTESIAN_POINT ( 'NONE',  ( -62.26794919243112503, 10.89508544963257464, 2.500000000000000000 ) ) ;
#8804 = CARTESIAN_POINT ( 'NONE',  ( -62.86468353124999453, 10.03645833299193413, 1.999225269531025750 ) ) ;
#8805 = CARTESIAN_POINT ( 'NONE',  ( -62.86468353124998742, 14.72395833299193413, 1.999225269531025972 ) ) ;
#8806 = CARTESIAN_POINT ( 'NONE',  ( -62.99999999999998579, 14.32291666598387003, 0.9226497308103756012 ) ) ;
#8807 = LINE ( 'NONE', #3033, #10712 ) ;
#8808 = EDGE_LOOP ( 'NONE', ( #10586, #4795, #1898, #10849 ) ) ;
#8809 = ORIENTED_EDGE ( 'NONE', *, *, #1848, .F. ) ;
#8810 = ADVANCED_FACE ( 'NONE', ( #3803 ), #6184, .T. ) ;
#8811 = CARTESIAN_POINT ( 'NONE',  ( -61.56765823437498852, 12.28645833299193413, 2.248837904296538515 ) ) ;
#8812 = CARTESIAN_POINT ( 'NONE',  ( -61.99999999999998579, 14.65624999931720041, 2.500000000000002665 ) ) ;
#8813 = CARTESIAN_POINT ( 'NONE',  ( -61.99999999999998579, 16.00000000000000000, 2.500000000000000444 ) ) ;
#8814 = ORIENTED_EDGE ( 'NONE', *, *, #6812, .T. ) ;
#8815 = CARTESIAN_POINT ( 'NONE',  ( -62.49999999999998579, 12.41666666666666607, 2.366025403784441483 ) ) ;
#8816 = CARTESIAN_POINT ( 'NONE',  ( -62.26794919243111082, 10.17633545031537068, 2.500000000000003109 ) ) ;
#8817 = CARTESIAN_POINT ( 'NONE',  ( -61.13531646874998415, 14.61979166632526805, 1.999225269531026417 ) ) ;
#8818 = LINE ( 'NONE', #1202, #10629 ) ;
#8819 = CARTESIAN_POINT ( 'NONE',  ( -60.99999999999998579, 11.19791666598387003, 2.077350269189628840 ) ) ;
#8820 = EDGE_LOOP ( 'NONE', ( #521, #6863, #10545, #6883 ) ) ;
#8821 = CARTESIAN_POINT ( 'NONE',  ( -61.99999999999998579, 16.00000000000000000, 1.500000000000002220 ) ) ;
#8822 = EDGE_CURVE ( 'NONE', #2668, #3478, #5334, .T. ) ;
#8823 = CARTESIAN_POINT ( 'NONE',  ( -61.99999999999998579, 14.31250000000000000, 0.5000000000000013323 ) ) ;
#8824 = CARTESIAN_POINT ( 'NONE',  ( -61.13531646874998415, 12.59895833299193590, 1.000774730468978468 ) ) ;
#8825 = EDGE_CURVE ( 'NONE', #7251, #1211, #6356, .T. ) ;
#8826 = CARTESIAN_POINT ( 'NONE',  ( -37.99999999999999289, -14.00000000000000888, -2.000000000000000000 ) ) ;
#8827 = ORIENTED_EDGE ( 'NONE', *, *, #3433, .F. ) ;
#8828 = CARTESIAN_POINT ( 'NONE',  ( -62.43234176562498305, 10.47395833299193413, 0.7511620957034662593 ) ) ;
#8829 =( BOUNDED_CURVE ( )  B_SPLINE_CURVE ( 2, ( #4569, #533, #8033, #10523, #3917, #7307, #9026, #3682, #9327 ),
 .UNSPECIFIED., .F., .T. ) 
 B_SPLINE_CURVE_WITH_KNOTS ( ( 3, 2, 2, 2, 3 ),
 ( 0.9765625000000000000, 0.9791666666666666297, 0.9843750000000000000, 0.9895833333333333703, 0.9921875000000000000 ),
 .UNSPECIFIED. ) 
 CURVE ( )  GEOMETRIC_REPRESENTATION_ITEM ( )  RATIONAL_B_SPLINE_CURVE ( ( 0.9330127018922194093, 0.9330127018922194093, 1.000000000000000000, 0.8660254037844387076, 1.000000000000000000, 0.8660254037844387076, 1.000000000000000000, 0.9330127018922194093, 0.9330127018922194093 ) ) 
 REPRESENTATION_ITEM ( '' )  );
#8830 = DIRECTION ( 'NONE',  ( 0.000000000000000000, 0.000000000000000000, -1.000000000000000000 ) ) ;
#8831 = CARTESIAN_POINT ( 'NONE',  ( -62.86468353124998032, 14.24479166632526983, 1.000774730468978246 ) ) ;
#8832 = CARTESIAN_POINT ( 'NONE',  ( 0.5000000000000000000, -0.2499999999999997780, -2.000000000000000000 ) ) ;
#8833 = VERTEX_POINT ( 'NONE', #8971 ) ;
#8834 = CARTESIAN_POINT ( 'NONE',  ( -76.99999999999998579, 11.49999999999999645, 5.000000000000000000 ) ) ;
#8835 = VERTEX_POINT ( 'NONE', #9802 ) ;
#8836 = CARTESIAN_POINT ( 'NONE',  ( -62.26794919243111082, 15.04241454900182973, 0.5000000000000013323 ) ) ;
#8837 = CARTESIAN_POINT ( 'NONE',  ( -62.86468353124998742, 15.97395833299193590, 1.999225269531025972 ) ) ;
#8838 = DIRECTION ( 'NONE',  ( -0.000000000000000000, -1.000000000000000000, -0.000000000000000000 ) ) ;
#8839 = CARTESIAN_POINT ( 'NONE',  ( -61.99999999999998579, 15.53124999931720041, 0.5000000000000013323 ) ) ;
#8840 = CARTESIAN_POINT ( 'NONE',  ( -61.99999999999998579, 10.78124999931720218, 0.5000000000000013323 ) ) ;
#8841 = CARTESIAN_POINT ( 'NONE',  ( -61.99999999999999289, 14.95312499965860198, 0.5015494609379544944 ) ) ;
#8842 = CARTESIAN_POINT ( 'NONE',  ( -61.56765823437498142, 10.11979166632526805, 0.7511620957034663704 ) ) ;
#8843 = CARTESIAN_POINT ( 'NONE',  ( -61.99999999999998579, 9.437499999999998224, 2.500000000000002665 ) ) ;
#8844 = VECTOR ( 'NONE', #8347, 1000.000000000000000 ) ;
#8845 = CARTESIAN_POINT ( 'NONE',  ( -62.86468353124999453, 11.01562499965860020, 1.500000000000002220 ) ) ;
#8846 = LINE ( 'NONE', #9620, #2180 ) ;
#8847 = ORIENTED_EDGE ( 'NONE', *, *, #9267, .T. ) ;
#8848 = ADVANCED_FACE ( 'NONE', ( #3676 ), #9743, .F. ) ;
#8849 = FACE_BOUND ( 'NONE', #1977, .T. ) ;
#8850 = UNCERTAINTY_MEASURE_WITH_UNIT (LENGTH_MEASURE( 1.000000000000000082E-05 ), #3469, 'distance_accuracy_value', 'NONE');
#8851 = CYLINDRICAL_SURFACE ( 'NONE', #6461, 20.00000000000000355 ) ;
#8852 = EDGE_CURVE ( 'NONE', #353, #7478, #10240, .T. ) ;
#8853 = ORIENTED_EDGE ( 'NONE', *, *, #3539, .F. ) ;
#8854 = CARTESIAN_POINT ( 'NONE',  ( -60.99999999999998579, 10.02083333333333215, 0.9226497308103762673 ) ) ;
#8855 = CARTESIAN_POINT ( 'NONE',  ( -62.86468353124998742, 12.72395833299193413, 1.999225269531025972 ) ) ;
#8856 = VECTOR ( 'NONE', #454, 1000.000000000000000 ) ;
#8857 = CARTESIAN_POINT ( 'NONE',  ( -61.13531646874997705, 9.807291666325268054, 1.999225269531026417 ) ) ;
#8858 = CARTESIAN_POINT ( 'NONE',  ( -61.99999999999998579, 16.00000000000000000, 2.500000000000000444 ) ) ;
#8859 = VERTEX_POINT ( 'NONE', #5451 ) ;
#8860 = CARTESIAN_POINT ( 'NONE',  ( -62.86468353124999453, 12.03645833299193413, 1.999225269531025750 ) ) ;
#8861 = APPLICATION_PROTOCOL_DEFINITION ( 'draft international standard', 'automotive_design', 1998, #1001 ) ;
#8862 = CARTESIAN_POINT ( 'NONE',  ( -62.43234176562498305, 15.66145833299193590, 0.7511620957034662593 ) ) ;
#8863 = EDGE_CURVE ( 'NONE', #3037, #6239, #3728, .T. ) ;
#8864 = CARTESIAN_POINT ( 'NONE',  ( -61.49999999999998579, 14.76041666598386826, 0.6339745962155628467 ) ) ;
#8865 = CARTESIAN_POINT ( 'NONE',  ( 0.000000000000000000, 0.000000000000000000, -2.000000000000000000 ) ) ;
#8866 = ORIENTED_EDGE ( 'NONE', *, *, #6873, .T. ) ;
#8867 = SHAPE_REPRESENTATION ( 'slotted pan head screw_iso_ISO 1580 - M2 x 10 - 10N', ( #2307 ), #6215 ) ;
#8868 = SURFACE_STYLE_USAGE ( .BOTH. , #8925 ) ;
#8869 = ORIENTED_EDGE ( 'NONE', *, *, #5058, .T. ) ;
#8870 = CARTESIAN_POINT ( 'NONE',  ( -62.86468353124999453, 12.97395833299193413, 1.999225269531025750 ) ) ;
#8871 = CARTESIAN_POINT ( 'NONE',  ( -61.13531646874998415, 9.078124999658601979, 1.500000000000002220 ) ) ;
#8872 = DIRECTION ( 'NONE',  ( -0.000000000000000000, -0.000000000000000000, -1.000000000000000000 ) ) ;
#8873 = VERTEX_POINT ( 'NONE', #5574 ) ;
#8874 = CARTESIAN_POINT ( 'NONE',  ( -61.49999999999998579, 12.29166666666666607, 0.6339745962155628467 ) ) ;
#8875 = CARTESIAN_POINT ( 'NONE',  ( -61.99999999999998579, 15.90624999931719863, 2.500000000000002665 ) ) ;
#8876 = AXIS2_PLACEMENT_3D ( 'NONE', #313, #2651, #4350 ) ;
#8877 = CARTESIAN_POINT ( 'NONE',  ( -62.43234176562498305, 14.47395833299193413, 0.7511620957034662593 ) ) ;
#8878 = SURFACE_STYLE_FILL_AREA ( #10477 ) ;
#8879 = CYLINDRICAL_SURFACE ( 'NONE', #10802, 0.9999999999999981126 ) ;
#8880 = CARTESIAN_POINT ( 'NONE',  ( -60.99999999999998579, 10.96874999931720218, 1.500000000000002220 ) ) ;
#8881 = ORIENTED_EDGE ( 'NONE', *, *, #3573, .T. ) ;
#8882 = FACE_OUTER_BOUND ( 'NONE', #1273, .T. ) ;
#8883 = VECTOR ( 'NONE', #5828, 1000.000000000000000 ) ;
#8884 = CARTESIAN_POINT ( 'NONE',  ( -62.43234176562498305, 12.91145833299193590, 0.7511620957034662593 ) ) ;
#8885 = EDGE_CURVE ( 'NONE', #1879, #4030, #1463, .T. ) ;
#8886 = CARTESIAN_POINT ( 'NONE',  ( 0.000000000000000000, 0.000000000000000000, 0.000000000000000000 ) ) ;
#8887 = AXIS2_PLACEMENT_3D ( 'NONE', #9277, #2550, #5203 ) ;
#8888 = VERTEX_POINT ( 'NONE', #3027 ) ;
#8889 = EDGE_CURVE ( 'NONE', #9315, #6452, #2916, .T. ) ;
#8890 = CARTESIAN_POINT ( 'NONE',  ( -61.99999999999998579, 10.32812499965860020, 2.498450539062049724 ) ) ;
#8891 = CARTESIAN_POINT ( 'NONE',  ( -25.39999999999996305, 1.224646799147353207E-16, -1.000000000000000000 ) ) ;
#8892 = CARTESIAN_POINT ( 'NONE',  ( -62.43234176562498305, 15.22395833299193590, 0.7511620957034662593 ) ) ;
#8893 = CARTESIAN_POINT ( 'NONE',  ( -144.9999999999999432, 8.000000000000000000, 0.000000000000000000 ) ) ;
#8894 = EDGE_LOOP ( 'NONE', ( #8827, #3185, #6207, #3351 ) ) ;
#8895 = CARTESIAN_POINT ( 'NONE',  ( -62.99999999999998579, 9.395833333333333925, 2.077350269189627952 ) ) ;
#8896 = ORIENTED_EDGE ( 'NONE', *, *, #9592, .F. ) ;
#8897 = CARTESIAN_POINT ( 'NONE',  ( -61.49999999999998579, 8.708333333333333925, 2.366025403784441927 ) ) ;
#8898 = CARTESIAN_POINT ( 'NONE',  ( -61.49999999999998579, 10.04166666666666785, 0.6339745962155628467 ) ) ;
#8899 = PLANE ( 'NONE',  #7881 ) ;
#8900 = CARTESIAN_POINT ( 'NONE',  ( -61.99999999999998579, 9.812500000000000000, 0.5000000000000013323 ) ) ;
#8901 = LINE ( 'NONE', #5317, #2275 ) ;
#8902 = CARTESIAN_POINT ( 'NONE',  ( -61.13531646874998415, 9.848958332991934128, 1.000774730468978468 ) ) ;
#8903 = LINE ( 'NONE', #9558, #7099 ) ;
#8904 = CARTESIAN_POINT ( 'NONE',  ( -61.99999999999998579, 16.00000000000000000, 1.500000000000002220 ) ) ;
#8905 = EDGE_CURVE ( 'NONE', #7083, #312, #7491, .T. ) ;
#8906 = CARTESIAN_POINT ( 'NONE',  ( -61.13531646874998415, 10.16145833299193413, 1.000774730468978468 ) ) ;
#8907 = CARTESIAN_POINT ( 'NONE',  ( -61.99999999999998579, 13.68749999999999822, 2.500000000000002665 ) ) ;
#8908 = EDGE_LOOP ( 'NONE', ( #7964, #5177, #10024, #7297, #5201, #4729, #5761, #9692 ) ) ;
#8909 = CARTESIAN_POINT ( 'NONE',  ( -61.99999999999998579, 13.40624999931720041, 2.500000000000002665 ) ) ;
#8910 = DIRECTION ( 'NONE',  ( -0.000000000000000000, -1.000000000000000000, -0.000000000000000000 ) ) ;
#8911 =( REPRESENTATION_RELATIONSHIP ('NONE','NONE', #560, #1195 ) REPRESENTATION_RELATIONSHIP_WITH_TRANSFORMATION ( #3229 )SHAPE_REPRESENTATION_RELATIONSHIP( ) );
#8912 = VERTEX_POINT ( 'NONE', #2391 ) ;
#8913 = CARTESIAN_POINT ( 'NONE',  ( -60.99999999999998579, 10.19791666598387181, 2.077350269189628840 ) ) ;
#8914 = CARTESIAN_POINT ( 'NONE',  ( -62.43234176562498305, 12.91145833299193590, 0.7511620957034662593 ) ) ;
#8915 = CARTESIAN_POINT ( 'NONE',  ( -61.99999999999999289, 9.765624999658600203, 2.498450539062049724 ) ) ;
#8916 = ORIENTED_EDGE ( 'NONE', *, *, #7132, .F. ) ;
#8917 = DIRECTION ( 'NONE',  ( 1.000000000000000000, 0.000000000000000000, 0.000000000000000000 ) ) ;
#8918 = CLOSED_SHELL ( 'NONE', ( #3373, #3106, #197, #8598, #2547, #4056, #7762, #2132, #7498, #614, #4738, #980, #10005 ) ) ;
#8919 = CARTESIAN_POINT ( 'NONE',  ( -61.13531646874997705, 11.61979166632526805, 1.999225269531026417 ) ) ;
#8920 = APPLICATION_PROTOCOL_DEFINITION ( 'draft international standard', 'automotive_design', 1998, #1935 ) ;
#8921 = CARTESIAN_POINT ( 'NONE',  ( -61.99999999999998579, 14.64062499965860020, 0.5015494609379544944 ) ) ;
#8922 = CARTESIAN_POINT ( 'NONE',  ( -60.99999999999998579, 14.46874999931720218, 1.500000000000002220 ) ) ;
#8923 = CARTESIAN_POINT ( 'NONE',  ( -61.73205080756886076, 14.77008544963257108, 0.5000000000000014433 ) ) ;
#8924 = ORIENTED_EDGE ( 'NONE', *, *, #2925, .T. ) ;
#8925 = SURFACE_SIDE_STYLE ('',( #6253 ) ) ;
#8926 = ORIENTED_EDGE ( 'NONE', *, *, #7864, .T. ) ;
#8927 = CARTESIAN_POINT ( 'NONE',  ( -61.99999999999999289, 13.14062499965860198, 0.5015494609379544944 ) ) ;
#8928 = CARTESIAN_POINT ( 'NONE',  ( -61.13531646874998415, 8.578124999658601979, 1.500000000000002220 ) ) ;
#8929 = CARTESIAN_POINT ( 'NONE',  ( -62.26794919243112503, 10.64508544963257464, 2.500000000000000000 ) ) ;
#8930 = ORIENTED_EDGE ( 'NONE', *, *, #6269, .T. ) ;
#8931 = CARTESIAN_POINT ( 'NONE',  ( -60.99999999999998579, 11.97916666666666785, 2.077350269189628840 ) ) ;
#8932 = CARTESIAN_POINT ( 'NONE',  ( -62.99999999999998579, 13.34374999931720396, 1.500000000000001998 ) ) ;
#8933 =( BOUNDED_CURVE ( )  B_SPLINE_CURVE ( 2, ( #9529, #1811, #4409, #138, #8643, #5414, #1922, #2701, #2875 ),
 .UNSPECIFIED., .F., .F. ) 
 B_SPLINE_CURVE_WITH_KNOTS ( ( 3, 2, 2, 2, 3 ),
 ( 0.2734375000000000000, 0.2760416666666666852, 0.2812500000000000000, 0.2864583333333333148, 0.2890624999999999445 ),
 .UNSPECIFIED. ) 
 CURVE ( )  GEOMETRIC_REPRESENTATION_ITEM ( )  RATIONAL_B_SPLINE_CURVE ( ( 0.9330127018922194093, 0.9330127018922194093, 1.000000000000000000, 0.8660254037844387076, 1.000000000000000000, 0.8660254037844387076, 1.000000000000000000, 0.9330127018922207416, 0.9330127018922192983 ) ) 
 REPRESENTATION_ITEM ( '' )  );
#8934 = CARTESIAN_POINT ( 'NONE',  ( -49.99999999999998579, -15.00000000000001243, 3.141811147483255962 ) ) ;
#8935 = CIRCLE ( 'NONE', #6971, 1.099999999999989875 ) ;
#8936 = AXIS2_PLACEMENT_3D ( 'NONE', #4806, #3983, #7373 ) ;
#8937 = CARTESIAN_POINT ( 'NONE',  ( -60.99999999999998579, 10.71874999931720396, 1.500000000000002220 ) ) ;
#8938 = ORIENTED_EDGE ( 'NONE', *, *, #572, .T. ) ;
#8939 = DIRECTION ( 'NONE',  ( -0.000000000000000000, 0.000000000000000000, 1.000000000000000000 ) ) ;
#8940 = VECTOR ( 'NONE', #3222, 1000.000000000000000 ) ;
#8941 = CARTESIAN_POINT ( 'NONE',  ( -62.43234176562499016, 12.49479166632526805, 2.248837904296538071 ) ) ;
#8942 = CYLINDRICAL_SURFACE ( 'NONE', #6349, 50.00000000000000000 ) ;
#8943 = VERTEX_POINT ( 'NONE', #4888 ) ;
#8944 = CARTESIAN_POINT ( 'NONE',  ( -62.43234176562499016, 11.30729166632526805, 2.248837904296538071 ) ) ;
#8945 = FACE_OUTER_BOUND ( 'NONE', #6515, .T. ) ;
#8946 = CIRCLE ( 'NONE', #242, 3.000000000000002665 ) ;
#8947 = CARTESIAN_POINT ( 'NONE',  ( -61.56765823437498852, 15.34895833299193590, 2.248837904296538515 ) ) ;
#8948 = CARTESIAN_POINT ( 'NONE',  ( -60.99999999999998579, 8.968749999317203958, 1.500000000000002220 ) ) ;
#8949 = ORIENTED_EDGE ( 'NONE', *, *, #8005, .F. ) ;
#8950 = CARTESIAN_POINT ( 'NONE',  ( -61.99999999999998579, 16.00000000000000000, 1.500000000000002220 ) ) ;
#8951 = ADVANCED_FACE ( 'NONE', ( #7303 ), #10840, .F. ) ;
#8952 = ORIENTED_EDGE ( 'NONE', *, *, #6602, .T. ) ;
#8953 = LINE ( 'NONE', #3892, #5172 ) ;
#8954 = CARTESIAN_POINT ( 'NONE',  ( -60.99999999999998579, 10.25000000000000000, 1.500000000000002220 ) ) ;
#8955 = FACE_OUTER_BOUND ( 'NONE', #1886, .T. ) ;
#8956 = CARTESIAN_POINT ( 'NONE',  ( -61.73205080756886076, 11.94866454968463110, 2.500000000000003109 ) ) ;
#8957 = FACE_OUTER_BOUND ( 'NONE', #7926, .T. ) ;
#8958 = CARTESIAN_POINT ( 'NONE',  ( -62.43234176562499016, 9.744791666325268054, 2.248837904296538071 ) ) ;
#8959 = CARTESIAN_POINT ( 'NONE',  ( -62.26794919243111082, 15.89508544963257108, 2.500000000000003109 ) ) ;
#8960 = CARTESIAN_POINT ( 'NONE',  ( -61.13531646874998415, 12.14062499965860198, 1.500000000000002220 ) ) ;
#8961 = DIRECTION ( 'NONE',  ( 0.000000000000000000, 1.065814103640150121E-14, 1.000000000000000000 ) ) ;
#8962 = ORIENTED_EDGE ( 'NONE', *, *, #6879, .F. ) ;
#8963 = CARTESIAN_POINT ( 'NONE',  ( 150.0000000000000284, -8.000000000000000000, 2.000000000000000000 ) ) ;
#8964 = DIRECTION ( 'NONE',  ( 0.000000000000000000, -1.000000000000000000, 0.000000000000000000 ) ) ;
#8965 = ORIENTED_EDGE ( 'NONE', *, *, #6578, .T. ) ;
#8966 = CARTESIAN_POINT ( 'NONE',  ( -62.49999999999998579, 10.38541666598387003, 2.366025403784441483 ) ) ;
#8967 = ADVANCED_FACE ( 'NONE', ( #3224, #9857 ), #2245, .T. ) ;
#8968 = CARTESIAN_POINT ( 'NONE',  ( -62.86468353124999453, 13.95312499965860198, 1.500000000000002220 ) ) ;
#8969 = CARTESIAN_POINT ( 'NONE',  ( -61.99999999999999289, 10.01562499965860198, 2.498450539062049724 ) ) ;
#8970 = ORIENTED_EDGE ( 'NONE', *, *, #4046, .T. ) ;
#8971 = CARTESIAN_POINT ( 'NONE',  ( -61.99999999999998579, 15.28124999931720218, 0.5000000000000013323 ) ) ;
#8972 = CARTESIAN_POINT ( 'NONE',  ( -61.13531646874998415, 11.39062499965860020, 1.500000000000002220 ) ) ;
#8973 = PRODUCT_CONTEXT ( 'NONE', #1001, 'mechanical' ) ;
#8974 = DIRECTION ( 'NONE',  ( -0.000000000000000000, -1.000000000000000000, -0.000000000000000000 ) ) ;
#8975 = CARTESIAN_POINT ( 'NONE',  ( -61.99999999999998579, 15.90624999931720396, 2.654700538379254571 ) ) ;
#8976 =( REPRESENTATION_RELATIONSHIP ('NONE','NONE', #560, #5800 ) REPRESENTATION_RELATIONSHIP_WITH_TRANSFORMATION ( #6529 )SHAPE_REPRESENTATION_RELATIONSHIP( ) );
#8977 = DIRECTION ( 'NONE',  ( 1.000000000000000000, 0.000000000000000000, 0.000000000000000000 ) ) ;
#8978 = VERTEX_POINT ( 'NONE', #9126 ) ;
#8979 = ORIENTED_EDGE ( 'NONE', *, *, #7699, .F. ) ;
#8980 = CARTESIAN_POINT ( 'NONE',  ( -62.43234176562498305, 12.91145833299193590, 0.7511620957034662593 ) ) ;
#8981 = CARTESIAN_POINT ( 'NONE',  ( -61.99999999999998579, 9.515624999658601979, 2.498450539062049724 ) ) ;
#8982 = CARTESIAN_POINT ( 'NONE',  ( -62.99999999999998579, 8.395833333333333925, 2.077350269189627952 ) ) ;
#8983 = EDGE_LOOP ( 'NONE', ( #3523, #3262, #9121, #6997 ) ) ;
#8984 = CARTESIAN_POINT ( 'NONE',  ( -60.99999999999998579, 12.97916666666666785, 2.077350269189628840 ) ) ;
#8985 = CARTESIAN_POINT ( 'NONE',  ( -62.99999999999998579, 13.32291666598387003, 0.9226497308103756012 ) ) ;
#8986 =( LENGTH_UNIT ( ) NAMED_UNIT ( * ) SI_UNIT ( .MILLI., .METRE. ) );
#8987 = CARTESIAN_POINT ( 'NONE',  ( -61.49999999999998579, 10.01041666598387003, 0.6339745962155628467 ) ) ;
#8988 = CARTESIAN_POINT ( 'NONE',  ( -9.277551871276348458E-15, -0.2500000000000001110, 1.454152683131083812 ) ) ;
#8989 = CARTESIAN_POINT ( 'NONE',  ( -61.56765823437498852, 13.28645833299193413, 2.248837904296538515 ) ) ;
#8990 = CARTESIAN_POINT ( 'NONE',  ( -61.99999999999998579, 8.312499999999998224, 0.5000000000000013323 ) ) ;
#8991 =( BOUNDED_CURVE ( )  B_SPLINE_CURVE ( 2, ( #6731, #7404, #7461, #10104, #8192, #10786, #5622, #2390, #3963 ),
 .UNSPECIFIED., .F., .T. ) 
 B_SPLINE_CURVE_WITH_KNOTS ( ( 3, 2, 2, 2, 3 ),
 ( 0.007812499999999973112, 0.01041666666666666609, 0.01562500000000000000, 0.02083333333333333218, 0.02343749999999996531 ),
 .UNSPECIFIED. ) 
 CURVE ( )  GEOMETRIC_REPRESENTATION_ITEM ( )  RATIONAL_B_SPLINE_CURVE ( ( 0.9330127018922194093, 0.9330127018922187432, 1.000000000000000000, 0.8660254037844387076, 1.000000000000000000, 0.8660254037844387076, 1.000000000000000000, 0.9330127018922202975, 0.9330127018922194093 ) ) 
 REPRESENTATION_ITEM ( '' )  );
#8992 = VERTEX_POINT ( 'NONE', #5681 ) ;
#8993 = CARTESIAN_POINT ( 'NONE',  ( -61.99999999999998579, 11.32812499965860020, 2.498450539062049724 ) ) ;
#8994 = CARTESIAN_POINT ( 'NONE',  ( -60.99999999999998579, 12.19791666598386826, 2.077350269189628840 ) ) ;
#8995 = EDGE_CURVE ( 'NONE', #1159, #6239, #5624, .T. ) ;
#8996 = CARTESIAN_POINT ( 'NONE',  ( -62.86468353124999453, 15.51562499965860198, 1.500000000000002220 ) ) ;
#8997 = ORIENTED_EDGE ( 'NONE', *, *, #8241, .T. ) ;
#8998 = CARTESIAN_POINT ( 'NONE',  ( -57.99999999999998579, -10.00000000000000888, 0.000000000000000000 ) ) ;
#8999 = ORIENTED_EDGE ( 'NONE', *, *, #10767, .T. ) ;
#9000 = CARTESIAN_POINT ( 'NONE',  ( -61.99999999999998579, 8.656249999317202182, 2.500000000000002665 ) ) ;
#9001 = CARTESIAN_POINT ( 'NONE',  ( -62.49999999999998579, 9.583333333333332149, 0.6339745962155627357 ) ) ;
#9002 = DIRECTION ( 'NONE',  ( 0.7071067811865439090, 8.659560562354888485E-17, -0.7071067811865512365 ) ) ;
#9003 = CARTESIAN_POINT ( 'NONE',  ( -104.9999999999999289, -15.00000000000001421, -2.000000000000000000 ) ) ;
#9004 = CARTESIAN_POINT ( 'NONE',  ( -61.99999999999998579, 8.187500000000001776, 2.500000000000003109 ) ) ;
#9005 = CARTESIAN_POINT ( 'NONE',  ( -44.00000000000000711, -14.00000000000000888, 0.000000000000000000 ) ) ;
#9006 = CARTESIAN_POINT ( 'NONE',  ( -62.86468353124998032, 12.49479166632526628, 1.000774730468978246 ) ) ;
#9007 = ORIENTED_EDGE ( 'NONE', *, *, #3592, .F. ) ;
#9008 = CARTESIAN_POINT ( 'NONE',  ( -60.99999999999998579, 9.239583332650536107, 0.9226497308103762673 ) ) ;
#9009 = FACE_OUTER_BOUND ( 'NONE', #8377, .T. ) ;
#9010 = VECTOR ( 'NONE', #6988, 1000.000000000000000 ) ;
#9011 = PRODUCT ( 'clamp', 'clamp', '', ( #4684 ) ) ;
#9012 = ORIENTED_EDGE ( 'NONE', *, *, #5754, .F. ) ;
#9013 = CARTESIAN_POINT ( 'NONE',  ( -61.99999999999998579, 14.15624999931720218, 2.500000000000002665 ) ) ;
#9014 = EDGE_CURVE ( 'NONE', #6754, #1879, #4862, .T. ) ;
#9015 = CARTESIAN_POINT ( 'NONE',  ( -62.43234176562499016, 14.24479166632526983, 2.248837904296538071 ) ) ;
#9016 = CARTESIAN_POINT ( 'NONE',  ( -61.99999999999999289, 9.890624999658601979, 0.5015494609379544944 ) ) ;
#9017 = DIRECTION ( 'NONE',  ( -0.000000000000000000, -1.000000000000000000, -0.000000000000000000 ) ) ;
#9018 = EDGE_LOOP ( 'NONE', ( #3870, #9585 ) ) ;
#9019 = CARTESIAN_POINT ( 'NONE',  ( -49.99999999999998579, -15.00000000000001243, -2.000000000000000000 ) ) ;
#9020 = CARTESIAN_POINT ( 'NONE',  ( -61.56765823437498142, 11.43229166632526805, 0.7511620957034663704 ) ) ;
#9021 = AXIS2_PLACEMENT_3D ( 'NONE', #3439, #4994, #2673 ) ;
#9022 = ADVANCED_FACE ( 'NONE', ( #4113 ), #3965, .T. ) ;
#9023 = CONTEXT_DEPENDENT_SHAPE_REPRESENTATION ( #4911, #5988 ) ;
#9024 = CARTESIAN_POINT ( 'NONE',  ( -25.39999999999996305, 1.224646799147353207E-16, -1.000000000000000000 ) ) ;
#9025 = CARTESIAN_POINT ( 'NONE',  ( -60.99999999999998579, 15.48958333265053788, 0.9226497308103762673 ) ) ;
#9026 = CARTESIAN_POINT ( 'NONE',  ( -62.49999999999998579, 16.13541666598386826, 2.366025403784441483 ) ) ;
#9027 = EDGE_LOOP ( 'NONE', ( #10591, #8595, #8051, #6558 ) ) ;
#9028 = FACE_OUTER_BOUND ( 'NONE', #9750, .T. ) ;
#9029 = DIRECTION ( 'NONE',  ( 0.000000000000000000, 0.000000000000000000, 1.000000000000000000 ) ) ;
#9030 = CARTESIAN_POINT ( 'NONE',  ( -61.13531646874998415, 14.57812499965860020, 1.500000000000002220 ) ) ;
#9031 = CARTESIAN_POINT ( 'NONE',  ( -61.56765823437498852, 10.28645833299193413, 2.248837904296538515 ) ) ;
#9032 = CIRCLE ( 'NONE', #9201, 1.000000000000000000 ) ;
#9033 = CARTESIAN_POINT ( 'NONE',  ( -61.99999999999998579, 16.00000000000000000, 2.500000000000000444 ) ) ;
#9034 = ORIENTED_EDGE ( 'NONE', *, *, #10288, .T. ) ;
#9035 = CARTESIAN_POINT ( 'NONE',  ( -60.99999999999998579, 14.27083333333333393, 0.9226497308103762673 ) ) ;
#9036 = FACE_OUTER_BOUND ( 'NONE', #1774, .T. ) ;
#9037 = FILL_AREA_STYLE_COLOUR ( '', #1584 ) ;
#9038 = VECTOR ( 'NONE', #3418, 1000.000000000000000 ) ;
#9039 = CARTESIAN_POINT ( 'NONE',  ( -62.99999999999998579, 11.36458333265053611, 2.077350269189627952 ) ) ;
#9040 = EDGE_CURVE ( 'NONE', #5032, #847, #6583, .T. ) ;
#9041 = VECTOR ( 'NONE', #6056, 1000.000000000000000 ) ;
#9042 = CARTESIAN_POINT ( 'NONE',  ( -62.99999999999998579, 14.87500000000000000, 1.500000000000001998 ) ) ;
#9043 = CARTESIAN_POINT ( 'NONE',  ( -61.13531646874998415, 12.07812499965860198, 1.500000000000002220 ) ) ;
#9044 = VECTOR ( 'NONE', #4169, 1000.000000000000000 ) ;
#9045 = VERTEX_POINT ( 'NONE', #731 ) ;
#9046 = CARTESIAN_POINT ( 'NONE',  ( -61.13531646874998415, 11.36979166632526628, 1.999225269531026417 ) ) ;
#9047 = ADVANCED_FACE ( 'NONE', ( #10894 ), #3284, .F. ) ;
#9048 = DIRECTION ( 'NONE',  ( 0.000000000000000000, 0.000000000000000000, 1.000000000000000000 ) ) ;
#9049 = AXIS2_PLACEMENT_3D ( 'NONE', #1297, #5443, #1120 ) ;
#9050 = CARTESIAN_POINT ( 'NONE',  ( -62.43234176562499016, 15.80729166632526628, 2.248837904296538071 ) ) ;
#9051 = ORIENTED_EDGE ( 'NONE', *, *, #1587, .F. ) ;
#9052 = EDGE_CURVE ( 'NONE', #6336, #40, #4010, .T. ) ;
#9053 = CARTESIAN_POINT ( 'NONE',  ( -77.99999999999998579, 11.49999999999999645, 8.000000000000000000 ) ) ;
#9054 = AXIS2_PLACEMENT_3D ( 'NONE', #126, #4456, #10400 ) ;
#9055 =( BOUNDED_CURVE ( )  B_SPLINE_CURVE ( 2, ( #3993, #9941, #6613, #561, #10723, #8118, #7282, #9992, #5762 ),
 .UNSPECIFIED., .F., .F. ) 
 B_SPLINE_CURVE_WITH_KNOTS ( ( 3, 2, 2, 2, 3 ),
 ( 0.3828125000000000000, 0.3854166666666666852, 0.3906250000000000000, 0.3958333333333333148, 0.3984375000000000000 ),
 .UNSPECIFIED. ) 
 CURVE ( )  GEOMETRIC_REPRESENTATION_ITEM ( )  RATIONAL_B_SPLINE_CURVE ( ( 0.9330127018922194093, 0.9330127018922194093, 1.000000000000000000, 0.8660254037844387076, 1.000000000000000000, 0.8660254037844387076, 1.000000000000000000, 0.9330127018922194093, 0.9330127018922194093 ) ) 
 REPRESENTATION_ITEM ( '' )  );
#9056 = ORIENTED_EDGE ( 'NONE', *, *, #5422, .F. ) ;
#9057 = CARTESIAN_POINT ( 'NONE',  ( 0.000000000000000000, 0.000000000000000000, 0.000000000000000000 ) ) ;
#9058 = EDGE_CURVE ( 'NONE', #7667, #8833, #2443, .T. ) ;
#9059 = CARTESIAN_POINT ( 'NONE',  ( -62.49999999999998579, 10.41666666666666785, 2.366025403784441483 ) ) ;
#9060 = VECTOR ( 'NONE', #3208, 1000.000000000000000 ) ;
#9061 = DIRECTION ( 'NONE',  ( -0.000000000000000000, -0.000000000000000000, -1.000000000000000000 ) ) ;
#9062 = DIRECTION ( 'NONE',  ( -0.000000000000000000, -1.000000000000000000, -0.000000000000000000 ) ) ;
#9063 = CARTESIAN_POINT ( 'NONE',  ( -62.49999999999998579, 14.88541666598386826, 2.366025403784441483 ) ) ;
#9064 = CARTESIAN_POINT ( 'NONE',  ( -60.99999999999998579, 8.489583332650536107, 0.9226497308103762673 ) ) ;
#9065 = CARTESIAN_POINT ( 'NONE',  ( -61.13531646874998415, 11.61979166632526983, 1.999225269531026417 ) ) ;
#9066 = CARTESIAN_POINT ( 'NONE',  ( -61.99999999999998579, 10.56249999999999822, 0.5000000000000013323 ) ) ;
#9067 = ORIENTED_EDGE ( 'NONE', *, *, #8852, .T. ) ;
#9068 = FACE_OUTER_BOUND ( 'NONE', #967, .T. ) ;
#9069 = DIRECTION ( 'NONE',  ( -0.000000000000000000, -0.000000000000000000, -1.000000000000000000 ) ) ;
#9070 = CARTESIAN_POINT ( 'NONE',  ( -77.99999999999998579, -11.50000000000000711, -2.000000000000001332 ) ) ;
#9071 = CARTESIAN_POINT ( 'NONE',  ( -62.86468353124999453, 14.45312499965860020, 1.500000000000002220 ) ) ;
#9072 = CARTESIAN_POINT ( 'NONE',  ( -61.56765823437498142, 9.869791666325268054, 0.7511620957034663704 ) ) ;
#9073 = PRESENTATION_STYLE_ASSIGNMENT (( #10054 ) ) ;
#9074 = CARTESIAN_POINT ( 'NONE',  ( -62.99999999999998579, 14.12499999999999822, 1.500000000000001998 ) ) ;
#9075 = CARTESIAN_POINT ( 'NONE',  ( -61.99999999999999289, 11.20312499965859843, 0.5015494609379544944 ) ) ;
#9076 = CARTESIAN_POINT ( 'NONE',  ( -62.43234176562499016, 16.05729166632526628, 2.248837904296538071 ) ) ;
#9077 = CONTEXT_DEPENDENT_SHAPE_REPRESENTATION ( #10945, #6886 ) ;
#9078 = CARTESIAN_POINT ( 'NONE',  ( -61.13531646874998415, 16.05729166632526983, 1.999225269531026417 ) ) ;
#9079 = CARTESIAN_POINT ( 'NONE',  ( -61.56765823437498142, 8.432291666325268054, 0.7511620957034663704 ) ) ;
#9080 = FACE_OUTER_BOUND ( 'NONE', #4830, .T. ) ;
#9081 = VERTEX_POINT ( 'NONE', #1363 ) ;
#9082 = CARTESIAN_POINT ( 'NONE',  ( -61.99999999999998579, 16.00000000000000000, 2.500000000000000444 ) ) ;
#9083 = DIRECTION ( 'NONE',  ( -1.000000000000000000, -1.734723475976807094E-15, 0.000000000000000000 ) ) ;
#9084 = EDGE_CURVE ( 'NONE', #3958, #7755, #8140, .T. ) ;
#9085 = AXIS2_PLACEMENT_3D ( 'NONE', #3395, #6852, #5275 ) ;
#9086 = CARTESIAN_POINT ( 'NONE',  ( -61.13531646874998415, 13.82812499965860198, 1.500000000000002220 ) ) ;
#9087 = CARTESIAN_POINT ( 'NONE',  ( -61.56765823437498852, 10.03645833299193413, 2.248837904296538515 ) ) ;
#9088 = LINE ( 'NONE', #2406, #2878 ) ;
#9089 = ORIENTED_EDGE ( 'NONE', *, *, #508, .T. ) ;
#9090 = CARTESIAN_POINT ( 'NONE',  ( -60.99999999999998579, 14.24999999999999822, 1.500000000000002220 ) ) ;
#9091 = CARTESIAN_POINT ( 'NONE',  ( -61.99999999999998579, 9.062500000000000000, 0.5000000000000013323 ) ) ;
#9092 = CARTESIAN_POINT ( 'NONE',  ( -62.49999999999998579, 12.38541666598386826, 2.366025403784441483 ) ) ;
#9093 = AXIS2_PLACEMENT_3D ( 'NONE', #10112, #10946, #1471 ) ;
#9094 = CARTESIAN_POINT ( 'NONE',  ( -62.43234176562498305, 14.41145833299193413, 0.7511620957034662593 ) ) ;
#9095 = DIRECTION ( 'NONE',  ( 0.000000000000000000, 0.000000000000000000, -1.000000000000000000 ) ) ;
#9096 = EDGE_LOOP ( 'NONE', ( #9646, #5776, #8267, #5984 ) ) ;
#9097 = VECTOR ( 'NONE', #4617, 1000.000000000000000 ) ;
#9098 = EDGE_CURVE ( 'NONE', #3792, #9204, #4730, .T. ) ;
#9099 = VECTOR ( 'NONE', #8641, 1000.000000000000000 ) ;
#9100 = CARTESIAN_POINT ( 'NONE',  ( -62.86468353124999453, 11.26562499965860020, 1.500000000000002220 ) ) ;
#9101 = CARTESIAN_POINT ( 'NONE',  ( -61.99999999999998579, 15.03124999931720218, 0.5000000000000013323 ) ) ;
#9102 = CARTESIAN_POINT ( 'NONE',  ( -61.13531646874998415, 15.66145833299193590, 1.000774730468978468 ) ) ;
#9103 = ORIENTED_EDGE ( 'NONE', *, *, #1371, .T. ) ;
#9104 = AXIS2_PLACEMENT_3D ( 'NONE', #1790, #8568, #7737 ) ;
#9105 = CARTESIAN_POINT ( 'NONE',  ( 150.0000000000000284, -8.000000000000000000, 3.000000000000000000 ) ) ;
#9106 = VERTEX_POINT ( 'NONE', #3078 ) ;
#9107 = CARTESIAN_POINT ( 'NONE',  ( -62.26794919243111082, 9.895085449632572860, 2.500000000000003109 ) ) ;
#9108 = CARTESIAN_POINT ( 'NONE',  ( -61.49999999999998579, 9.541666666666667851, 0.6339745962155628467 ) ) ;
#9109 = DIRECTION ( 'NONE',  ( 1.000000000000000000, 0.000000000000000000, 0.000000000000000000 ) ) ;
#9110 = CARTESIAN_POINT ( 'NONE',  ( -61.73205080756886076, 15.02008544963257108, 0.5000000000000014433 ) ) ;
#9111 = PLANE ( 'NONE',  #7078 ) ;
#9112 = CIRCLE ( 'NONE', #3249, 0.5999999999999999778 ) ;
#9113 = CYLINDRICAL_SURFACE ( 'NONE', #4406, 0.9999999999999981126 ) ;
#9114 = CARTESIAN_POINT ( 'NONE',  ( -61.99999999999998579, 11.70312499965860020, 0.5015494609379544944 ) ) ;
#9115 = CARTESIAN_POINT ( 'NONE',  ( -62.26794919243111082, 9.042414549001833279, 0.4999999999999998890 ) ) ;
#9116 = ORIENTED_EDGE ( 'NONE', *, *, #6084, .F. ) ;
#9117 =( BOUNDED_CURVE ( )  B_SPLINE_CURVE ( 2, ( #9066, #7453, #4103, #6622, #6671, #4829, #7502, #8236, #10885 ),
 .UNSPECIFIED., .F., .F. ) 
 B_SPLINE_CURVE_WITH_KNOTS ( ( 3, 2, 2, 2, 3 ),
 ( 0.3203125000000000000, 0.3229166666666666852, 0.3281250000000000000, 0.3333333333333333148, 0.3359374999999999445 ),
 .UNSPECIFIED. ) 
 CURVE ( )  GEOMETRIC_REPRESENTATION_ITEM ( )  RATIONAL_B_SPLINE_CURVE ( ( 0.9330127018922194093, 0.9330127018922194093, 1.000000000000000000, 0.8660254037844387076, 1.000000000000000000, 0.8660254037844387076, 1.000000000000000000, 0.9330127018922207416, 0.9330127018922192983 ) ) 
 REPRESENTATION_ITEM ( '' )  );
#9118 = CARTESIAN_POINT ( 'NONE',  ( -57.99999999999998579, -10.00000000000000888, 3.000000000000000000 ) ) ;
#9119 = EDGE_CURVE ( 'NONE', #8372, #5268, #10544, .T. ) ;
#9120 = AXIS2_PLACEMENT_3D ( 'NONE', #629, #9960, #1511 ) ;
#9121 = ORIENTED_EDGE ( 'NONE', *, *, #10836, .F. ) ;
#9122 = CARTESIAN_POINT ( 'NONE',  ( -61.99999999999998579, 16.00000000000000000, 1.500000000000002220 ) ) ;
#9123 = CARTESIAN_POINT ( 'NONE',  ( -61.99999999999998579, 13.26562499965860198, 2.498450539062049724 ) ) ;
#9124 = CARTESIAN_POINT ( 'NONE',  ( -60.99999999999998579, 13.75000000000000000, 1.500000000000002220 ) ) ;
#9125 = CARTESIAN_POINT ( 'NONE',  ( -60.99999999999998579, 14.47916666666666607, 2.077350269189628840 ) ) ;
#9126 = CARTESIAN_POINT ( 'NONE',  ( 0.5000000000000000000, -0.2499999999999997224, -1.911797424705720116 ) ) ;
#9127 = CARTESIAN_POINT ( 'NONE',  ( -61.13531646874998415, 12.89062499965860198, 1.500000000000002220 ) ) ;
#9128 = CARTESIAN_POINT ( 'NONE',  ( -61.13531646874998415, 15.89062499965860198, 1.500000000000002220 ) ) ;
#9129 = LINE ( 'NONE', #1516, #2827 ) ;
#9130 = CARTESIAN_POINT ( 'NONE',  ( -149.9999999999999716, 8.000000000000000000, 0.000000000000000000 ) ) ;
#9131 = CARTESIAN_POINT ( 'NONE',  ( -60.99999999999998579, 15.44791666598386826, 2.077350269189628840 ) ) ;
#9132 = CARTESIAN_POINT ( 'NONE',  ( 1.299999999999999156, 0.000000000000000000, 0.000000000000000000 ) ) ;
#9133 = ORIENTED_EDGE ( 'NONE', *, *, #5007, .T. ) ;
#9134 = DIRECTION ( 'NONE',  ( -0.000000000000000000, -0.000000000000000000, -1.000000000000000000 ) ) ;
#9135 = EDGE_CURVE ( 'NONE', #10734, #5253, #10265, .T. ) ;
#9136 = CARTESIAN_POINT ( 'NONE',  ( -1.478538361079743326E-14, 0.2499999999999997780, -1.453737367178235651 ) ) ;
#9137 = CARTESIAN_POINT ( 'NONE',  ( -61.56765823437498852, 14.78645833299193413, 2.248837904296538515 ) ) ;
#9138 = CARTESIAN_POINT ( 'NONE',  ( -62.43234176562499016, 9.494791666325268054, 2.248837904296538071 ) ) ;
#9139 = CARTESIAN_POINT ( 'NONE',  ( -62.86468353124998032, 15.74479166632526628, 1.000774730468978024 ) ) ;
#9140 = PLANE ( 'NONE',  #6246 ) ;
#9141 = ORIENTED_EDGE ( 'NONE', *, *, #5613, .F. ) ;
#9142 = CARTESIAN_POINT ( 'NONE',  ( -62.49999999999998579, 13.83333333333333215, 0.6339745962155627357 ) ) ;
#9143 = PLANE ( 'NONE',  #8936 ) ;
#9144 =( NAMED_UNIT ( * ) SI_UNIT ( $, .STERADIAN. ) SOLID_ANGLE_UNIT ( ) );
#9145 = CARTESIAN_POINT ( 'NONE',  ( -60.99999999999998579, 11.94791666598387181, 2.077350269189628840 ) ) ;
#9146 = ADVANCED_FACE ( 'NONE', ( #10325 ), #9233, .T. ) ;
#9147 = CARTESIAN_POINT ( 'NONE',  ( -61.99999999999998579, 9.562500000000000000, 0.5000000000000013323 ) ) ;
#9148 = CARTESIAN_POINT ( 'NONE',  ( -61.13531646874998415, 14.57812499965860020, 1.500000000000002220 ) ) ;
#9149 = CARTESIAN_POINT ( 'NONE',  ( -114.9999999999999147, -43.00000000000000000, 0.000000000000000000 ) ) ;
#9150 = ORIENTED_EDGE ( 'NONE', *, *, #3313, .F. ) ;
#9151 = ADVANCED_FACE ( 'NONE', ( #4370 ), #939, .F. ) ;
#9152 = CARTESIAN_POINT ( 'NONE',  ( -62.43234176562498305, 11.47395833299193590, 0.7511620957034662593 ) ) ;
#9153 = CARTESIAN_POINT ( 'NONE',  ( -61.99999999999998579, 12.28124999931720041, 0.5000000000000013323 ) ) ;
#9154 = ADVANCED_FACE ( 'NONE', ( #8398 ), #9439, .F. ) ;
#9155 = PLANE ( 'NONE',  #1936 ) ;
#9156 = VERTEX_POINT ( 'NONE', #5996 ) ;
#9157 = FACE_OUTER_BOUND ( 'NONE', #4480, .T. ) ;
#9158 = EDGE_CURVE ( 'NONE', #2837, #4305, #6365, .T. ) ;
#9159 = ORIENTED_EDGE ( 'NONE', *, *, #8113, .F. ) ;
#9160 = CARTESIAN_POINT ( 'NONE',  ( -61.99999999999998579, 8.531249999317203958, 0.5000000000000013323 ) ) ;
#9161 = CARTESIAN_POINT ( 'NONE',  ( -61.49999999999998579, 10.54166666666666607, 0.6339745962155628467 ) ) ;
#9162 = DIRECTION ( 'NONE',  ( -0.000000000000000000, -1.000000000000000000, -0.000000000000000000 ) ) ;
#9163 = DIRECTION ( 'NONE',  ( -0.000000000000000000, -1.000000000000000000, -0.000000000000000000 ) ) ;
#9164 = UNCERTAINTY_MEASURE_WITH_UNIT (LENGTH_MEASURE( 1.000000000000000082E-05 ), #897, 'distance_accuracy_value', 'NONE');
#9165 = CARTESIAN_POINT ( 'NONE',  ( -60.99999999999998579, 9.447916665983868256, 2.077350269189628840 ) ) ;
#9166 = CARTESIAN_POINT ( 'NONE',  ( -62.86468353124999453, 11.51562499965860020, 1.500000000000002220 ) ) ;
#9167 = DIRECTION ( 'NONE',  ( 0.000000000000000000, 0.000000000000000000, 1.000000000000000000 ) ) ;
#9168 = ORIENTED_EDGE ( 'NONE', *, *, #9950, .T. ) ;
#9169 = CARTESIAN_POINT ( 'NONE',  ( -62.99999999999998579, 15.37500000000000000, 1.500000000000001998 ) ) ;
#9170 = ORIENTED_EDGE ( 'NONE', *, *, #6868, .T. ) ;
#9171 = CYLINDRICAL_SURFACE ( 'NONE', #10868, 0.9999999999999981126 ) ;
#9172 = CARTESIAN_POINT ( 'NONE',  ( -62.43234176562499016, 13.74479166632526805, 2.248837904296538071 ) ) ;
#9173 = DIRECTION ( 'NONE',  ( -0.000000000000000000, -0.000000000000000000, 1.000000000000000000 ) ) ;
#9174 = CARTESIAN_POINT ( 'NONE',  ( 0.5000000000000000000, 0.000000000000000000, 0.000000000000000000 ) ) ;
#9175 = CARTESIAN_POINT ( 'NONE',  ( -62.99999999999998579, 8.343749999317202182, 1.500000000000001998 ) ) ;
#9176 = CARTESIAN_POINT ( 'NONE',  ( -61.56765823437498852, 13.34895833299193413, 2.248837904296538515 ) ) ;
#9177 = CARTESIAN_POINT ( 'NONE',  ( -61.99999999999998579, 15.07812499965860198, 2.498450539062049724 ) ) ;
#9178 = LINE ( 'NONE', #2157, #8674 ) ;
#9179 =( BOUNDED_CURVE ( )  B_SPLINE_CURVE ( 2, ( #546, #5590, #6543, #3196, #7263, #9760, #5696, #2156, #9091 ),
 .UNSPECIFIED., .F., .T. ) 
 B_SPLINE_CURVE_WITH_KNOTS ( ( 3, 2, 2, 2, 3 ),
 ( 0.1171875000000000278, 0.1197916666666666713, 0.1250000000000000000, 0.1302083333333333426, 0.1328125000000000000 ),
 .UNSPECIFIED. ) 
 CURVE ( )  GEOMETRIC_REPRESENTATION_ITEM ( )  RATIONAL_B_SPLINE_CURVE ( ( 0.9330127018922194093, 0.9330127018922200755, 1.000000000000000000, 0.8660254037844387076, 1.000000000000000000, 0.8660254037844387076, 1.000000000000000000, 0.9330127018922194093, 0.9330127018922194093 ) ) 
 REPRESENTATION_ITEM ( '' )  );
#9180 = APPLICATION_PROTOCOL_DEFINITION ( 'draft international standard', 'automotive_design', 1998, #10377 ) ;
#9181 = FACE_OUTER_BOUND ( 'NONE', #10404, .T. ) ;
#9182 = MECHANICAL_DESIGN_GEOMETRIC_PRESENTATION_REPRESENTATION (  '', ( #4910 ), #5089 ) ;
#9183 = CARTESIAN_POINT ( 'NONE',  ( -62.99999999999998579, 16.07291666598386826, 0.9226497308103756012 ) ) ;
#9184 = CYLINDRICAL_SURFACE ( 'NONE', #7664, 0.9999999999999981126 ) ;
#9185 = ORIENTED_EDGE ( 'NONE', *, *, #4732, .F. ) ;
#9186 = CARTESIAN_POINT ( 'NONE',  ( 0.000000000000000000, 0.000000000000000000, 3.000000000000000000 ) ) ;
#9187 = CARTESIAN_POINT ( 'NONE',  ( -77.99999999999998579, 0.000000000000000000, 13.00000000000000178 ) ) ;
#9188 = ADVANCED_FACE ( 'NONE', ( #9385 ), #7728, .T. ) ;
#9189 = CARTESIAN_POINT ( 'NONE',  ( -61.56765823437498142, 14.11979166632526805, 0.7511620957034663704 ) ) ;
#9190 = CARTESIAN_POINT ( 'NONE',  ( -61.56765823437498142, 9.869791666325268054, 0.7511620957034663704 ) ) ;
#9191 = AXIS2_PLACEMENT_3D ( 'NONE', #7322, #9984, #4810 ) ;
#9192 = CARTESIAN_POINT ( 'NONE',  ( -61.99999999999999289, 15.45312499965860020, 0.5015494609379544944 ) ) ;
#9193 = CARTESIAN_POINT ( 'NONE',  ( -61.99999999999998579, 14.40624999931720218, 2.500000000000002665 ) ) ;
#9194 = ORIENTED_EDGE ( 'NONE', *, *, #2423, .T. ) ;
#9195 = CARTESIAN_POINT ( 'NONE',  ( -62.99999999999998579, 13.39583333333333393, 2.077350269189627952 ) ) ;
#9196 = PRODUCT_DEFINITION_SHAPE ( 'NONE', 'NONE',  #8478 ) ;
#9197 = ADVANCED_FACE ( 'NONE', ( #7562 ), #5209, .F. ) ;
#9198 = CARTESIAN_POINT ( 'NONE',  ( -61.56765823437498852, 9.098958332991935904, 2.248837904296538515 ) ) ;
#9199 = CARTESIAN_POINT ( 'NONE',  ( -61.99999999999998579, 11.78124999931720218, 0.3452994616207497591 ) ) ;
#9200 = VECTOR ( 'NONE', #8178, 1000.000000000000000 ) ;
#9201 = AXIS2_PLACEMENT_3D ( 'NONE', #9495, #7952, #7120 ) ;
#9202 = CARTESIAN_POINT ( 'NONE',  ( -62.86468353124999453, 13.95312499965860198, 1.500000000000002220 ) ) ;
#9203 = PLANE ( 'NONE',  #3316 ) ;
#9204 = VERTEX_POINT ( 'NONE', #5890 ) ;
#9205 = VECTOR ( 'NONE', #5666, 1000.000000000000000 ) ;
#9206 = CARTESIAN_POINT ( 'NONE',  ( -61.99999999999998579, 12.45312499965860020, 0.5015494609379544944 ) ) ;
#9207 = CYLINDRICAL_SURFACE ( 'NONE', #10084, 0.9999999999999981126 ) ;
#9208 = LINE ( 'NONE', #1595, #8680 ) ;
#9209 = VERTEX_POINT ( 'NONE', #5047 ) ;
#9210 = DIRECTION ( 'NONE',  ( 0.000000000000000000, -0.000000000000000000, 1.000000000000000000 ) ) ;
#9211 = EDGE_CURVE ( 'NONE', #312, #5388, #1838, .T. ) ;
#9212 = AXIS2_PLACEMENT_3D ( 'NONE', #1230, #6114, #3665 ) ;
#9213 = EDGE_CURVE ( 'NONE', #10197, #6498, #991, .T. ) ;
#9214 = COLOUR_RGB ( '',0.8941176470588234615, 0.8941176470588234615, 0.8941176470588234615 ) ;
#9215 = ORIENTED_EDGE ( 'NONE', *, *, #9484, .F. ) ;
#9216 = CARTESIAN_POINT ( 'NONE',  ( -60.99999999999998579, 15.47916666666666607, 2.077350269189628840 ) ) ;
#9217 = CARTESIAN_POINT ( 'NONE',  ( -61.99999999999998579, 11.31250000000000000, 0.3452994616207497591 ) ) ;
#9218 = ORIENTED_EDGE ( 'NONE', *, *, #6350, .T. ) ;
#9219 = CARTESIAN_POINT ( 'NONE',  ( -61.49999999999998579, 14.92708333265053611, 2.366025403784441927 ) ) ;
#9220 = CARTESIAN_POINT ( 'NONE',  ( -62.99999999999998579, 13.84374999931720218, 1.500000000000001998 ) ) ;
#9221 = VECTOR ( 'NONE', #6268, 1000.000000000000000 ) ;
#9222 = CARTESIAN_POINT ( 'NONE',  ( -61.13531646874998415, 12.61979166632526805, 1.999225269531026417 ) ) ;
#9223 = AXIS2_PLACEMENT_3D ( 'NONE', #4391, #6187, #3399 ) ;
#9224 = CARTESIAN_POINT ( 'NONE',  ( -61.99999999999998579, 9.031249999317202182, 0.5000000000000013323 ) ) ;
#9225 = ORIENTED_EDGE ( 'NONE', *, *, #8822, .F. ) ;
#9226 = DIRECTION ( 'NONE',  ( 0.000000000000000000, 0.000000000000000000, -1.000000000000000000 ) ) ;
#9227 = AXIS2_PLACEMENT_3D ( 'NONE', #9731, #4444, #7905 ) ;
#9228 = ORIENTED_EDGE ( 'NONE', *, *, #1587, .T. ) ;
#9229 = CARTESIAN_POINT ( 'NONE',  ( -134.9999999999999147, 8.000000000000000000, 0.000000000000000000 ) ) ;
#9230 = CARTESIAN_POINT ( 'NONE',  ( -61.56765823437498142, 15.61979166632526628, 0.7511620957034663704 ) ) ;
#9231 = FACE_OUTER_BOUND ( 'NONE', #49, .T. ) ;
#9232 = CARTESIAN_POINT ( 'NONE',  ( -60.99999999999998579, 10.44791666598387003, 2.077350269189628840 ) ) ;
#9233 = CYLINDRICAL_SURFACE ( 'NONE', #5461, 0.9999999999999981126 ) ;
#9234 = CARTESIAN_POINT ( 'NONE',  ( -62.43234176562498305, 12.22395833299193413, 0.7511620957034662593 ) ) ;
#9235 = EDGE_CURVE ( 'NONE', #5087, #10857, #2958, .T. ) ;
#9236 = CARTESIAN_POINT ( 'NONE',  ( -62.86468353124999453, 15.51562499965860198, 1.500000000000002220 ) ) ;
#9237 = CARTESIAN_POINT ( 'NONE',  ( -61.73205080756886076, 14.94866454968462932, 2.500000000000003109 ) ) ;
#9238 = CARTESIAN_POINT ( 'NONE',  ( 146.0000000000000284, 5.500000000000000000, 3.000000000000000000 ) ) ;
#9239 = CARTESIAN_POINT ( 'NONE',  ( -61.99999999999998579, 8.828124999658601979, 2.498450539062049724 ) ) ;
#9240 = CARTESIAN_POINT ( 'NONE',  ( -62.99999999999998579, 10.35416666666666785, 0.9226497308103756012 ) ) ;
#9241 = ORIENTED_EDGE ( 'NONE', *, *, #10731, .F. ) ;
#9242 = DIRECTION ( 'NONE',  ( -1.000000000000000000, 0.000000000000000000, -0.000000000000000000 ) ) ;
#9243 = CARTESIAN_POINT ( 'NONE',  ( 0.05011565059742421196, 0.2499999999999998890, -1.595010514166263382 ) ) ;
#9244 = CARTESIAN_POINT ( 'NONE',  ( -62.86468353124999453, 13.95312499965860198, 1.500000000000002220 ) ) ;
#9245 = CARTESIAN_POINT ( 'NONE',  ( -61.99999999999998579, 10.76562499965860020, 2.498450539062049724 ) ) ;
#9246 = CARTESIAN_POINT ( 'NONE',  ( -62.86468353124998032, 8.182291666325268054, 1.000774730468978024 ) ) ;
#9247 = DIRECTION ( 'NONE',  ( 1.000000000000000000, 0.000000000000000000, 0.000000000000000000 ) ) ;
#9248 = EDGE_LOOP ( 'NONE', ( #10796, #9753, #3591, #4024, #8628, #5568, #2304, #9833, #765, #329, #6505, #2877, #6954, #7695, #5416, #8634, #10722, #1716, #183, #3466, #2787, #2590, #5082, #3902, #2883, #4675, #172, #9303, #4420, #3918, #3652, #9549, #5025, #8355, #6484, #7503, #8119, #188, #3811, #1667, #807, #7970, #3311, #7106, #2425, #6611, #1704, #7369, #8304, #6715, #10737, #3543, #6931, #7587, #9886, #6191, #5064, #2760, #1543, #2133, #1541, #3907, #1832, #10616, #659, #3307, #3169, #1496 ) ) ;
#9249 = CARTESIAN_POINT ( 'NONE',  ( -61.99999999999998579, 13.31250000000000000, 0.3452994616207497591 ) ) ;
#9250 = CARTESIAN_POINT ( 'NONE',  ( -61.13531646874998415, 8.390624999658601979, 1.500000000000002220 ) ) ;
#9251 = CARTESIAN_POINT ( 'NONE',  ( -62.99999999999998579, 12.09374999931720218, 1.500000000000001998 ) ) ;
#9252 = CARTESIAN_POINT ( 'NONE',  ( -60.99999999999998579, 9.479166666666669627, 2.077350269189628840 ) ) ;
#9253 = CIRCLE ( 'NONE', #5335, 1.000000000000000888 ) ;
#9254 = EDGE_CURVE ( 'NONE', #5880, #7919, #10893, .T. ) ;
#9255 = CARTESIAN_POINT ( 'NONE',  ( -61.56765823437498852, 13.53645833299193413, 2.248837904296538515 ) ) ;
#9256 = PRESENTATION_STYLE_ASSIGNMENT (( #3256 ) ) ;
#9257 = ORIENTED_EDGE ( 'NONE', *, *, #9877, .F. ) ;
#9258 = CARTESIAN_POINT ( 'NONE',  ( -61.56765823437498142, 13.43229166632526805, 0.7511620957034663704 ) ) ;
#9259 = CARTESIAN_POINT ( 'NONE',  ( -62.26794919243111082, 12.64508544963257286, 2.500000000000003109 ) ) ;
#9260 = CIRCLE ( 'NONE', #8733, 1.336466033005844434 ) ;
#9261 = PRODUCT_DEFINITION_CONTEXT ( 'detailed design', #4191, 'design' ) ;
#9262 = FACE_OUTER_BOUND ( 'NONE', #7308, .T. ) ;
#9263 = VERTEX_POINT ( 'NONE', #1947 ) ;
#9264 = CARTESIAN_POINT ( 'NONE',  ( -61.99999999999998579, 16.00000000000000000, 2.500000000000000444 ) ) ;
#9265 = VERTEX_POINT ( 'NONE', #8786 ) ;
#9266 = CARTESIAN_POINT ( 'NONE',  ( -61.99999999999998579, 11.06250000000000000, 0.3452994616207497591 ) ) ;
#9267 = EDGE_CURVE ( 'NONE', #8912, #3585, #8901, .T. ) ;
#9268 = ORIENTED_EDGE ( 'NONE', *, *, #5169, .F. ) ;
#9269 = CARTESIAN_POINT ( 'NONE',  ( -61.99999999999998579, 9.203124999658601979, 0.5015494609379544944 ) ) ;
#9270 = CARTESIAN_POINT ( 'NONE',  ( -61.49999999999998579, 10.51041666598387003, 0.6339745962155628467 ) ) ;
#9271 = SHAPE_REPRESENTATION ( 'fine adjustment wheel', ( #2307 ), #5679 ) ;
#9272 = VECTOR ( 'NONE', #1600, 1000.000000000000000 ) ;
#9273 = CARTESIAN_POINT ( 'NONE',  ( -62.86468353124998032, 12.74479166632526805, 1.000774730468978246 ) ) ;
#9274 = EDGE_CURVE ( 'NONE', #2941, #6452, #7175, .T. ) ;
#9275 = CARTESIAN_POINT ( 'NONE',  ( -62.26794919243111082, 12.89508544963257108, 2.500000000000003109 ) ) ;
#9276 = ORIENTED_EDGE ( 'NONE', *, *, #4087, .T. ) ;
#9277 = CARTESIAN_POINT ( 'NONE',  ( -77.99999999999998579, -11.50000000000000711, -2.000000000000000000 ) ) ;
#9278 = ORIENTED_EDGE ( 'NONE', *, *, #801, .F. ) ;
#9279 = CARTESIAN_POINT ( 'NONE',  ( 0.5000000000000000000, -0.2499999999999997224, -2.000000000000000000 ) ) ;
#9280 = CARTESIAN_POINT ( 'NONE',  ( -62.86468353124998032, 14.93229166632526983, 1.000774730468978246 ) ) ;
#9281 = CARTESIAN_POINT ( 'NONE',  ( -61.99999999999998579, 14.40624999931720218, 2.500000000000002665 ) ) ;
#9282 = CARTESIAN_POINT ( 'NONE',  ( 190.0000000000000000, -6.123233995736783046E-16, 4.000000000000000000 ) ) ;
#9283 = CARTESIAN_POINT ( 'NONE',  ( -61.99999999999998579, 16.00000000000000000, 1.500000000000002220 ) ) ;
#9284 = CARTESIAN_POINT ( 'NONE',  ( -62.86468353124999453, 13.28645833299193413, 1.999225269531025750 ) ) ;
#9285 = CARTESIAN_POINT ( 'NONE',  ( -62.43234176562498305, 8.161458332991934128, 0.7511620957034662593 ) ) ;
#9286 = CYLINDRICAL_SURFACE ( 'NONE', #4766, 0.9999999999999981126 ) ;
#9287 = DIRECTION ( 'NONE',  ( -0.000000000000000000, -1.000000000000000000, -0.000000000000000000 ) ) ;
#9288 = CARTESIAN_POINT ( 'NONE',  ( -61.13531646874998415, 9.140624999658601979, 1.500000000000002220 ) ) ;
#9289 = CARTESIAN_POINT ( 'NONE',  ( -61.99999999999998579, 10.65624999931720218, 2.500000000000002665 ) ) ;
#9290 = ORIENTED_EDGE ( 'NONE', *, *, #3250, .F. ) ;
#9291 = AXIS2_PLACEMENT_3D ( 'NONE', #9552, #1109, #7780 ) ;
#9292 = DIRECTION ( 'NONE',  ( -0.000000000000000000, 1.000000000000000000, -0.000000000000000000 ) ) ;
#9293 = DIRECTION ( 'NONE',  ( 1.734723475976807094E-15, -1.000000000000000000, 0.000000000000000000 ) ) ;
#9294 = EDGE_CURVE ( 'NONE', #9906, #8873, #8486, .T. ) ;
#9295 = CARTESIAN_POINT ( 'NONE',  ( -109.9999999999999432, 14.99999999999998579, 0.000000000000000000 ) ) ;
#9296 = CARTESIAN_POINT ( 'NONE',  ( -61.13531646874998415, 11.30729166632526805, 1.999225269531026417 ) ) ;
#9297 = CARTESIAN_POINT ( 'NONE',  ( -62.86468353124999453, 15.01562499965860020, 1.500000000000002220 ) ) ;
#9298 = DIRECTION ( 'NONE',  ( -0.8660254037844418162, -0.4999999999999947264, 0.000000000000000000 ) ) ;
#9299 = ORIENTED_EDGE ( 'NONE', *, *, #153, .T. ) ;
#9300 = CARTESIAN_POINT ( 'NONE',  ( -61.49999999999998579, 14.95833333333333393, 2.366025403784441927 ) ) ;
#9301 = CARTESIAN_POINT ( 'NONE',  ( -62.86468353124999453, 9.036458332991935904, 1.999225269531025750 ) ) ;
#9302 = CARTESIAN_POINT ( 'NONE',  ( -62.99999999999998579, 12.86458333265053788, 2.077350269189627952 ) ) ;
#9303 = ORIENTED_EDGE ( 'NONE', *, *, #2766, .T. ) ;
#9304 = CARTESIAN_POINT ( 'NONE',  ( -62.43234176562499016, 14.24479166632526983, 2.248837904296538071 ) ) ;
#9305 = CARTESIAN_POINT ( 'NONE',  ( -61.99999999999998579, 16.00000000000000000, 1.500000000000002220 ) ) ;
#9306 = VERTEX_POINT ( 'NONE', #7230 ) ;
#9307 = CYLINDRICAL_SURFACE ( 'NONE', #4308, 1.099999999999989875 ) ;
#9308 = CARTESIAN_POINT ( 'NONE',  ( -61.99999999999998579, 13.20312499965860198, 0.5015494609379544944 ) ) ;
#9309 = CARTESIAN_POINT ( 'NONE',  ( -61.99999999999998579, 12.65624999931720396, 2.500000000000002665 ) ) ;
#9310 = VERTEX_POINT ( 'NONE', #4608 ) ;
#9311 = LINE ( 'NONE', #2589, #7803 ) ;
#9312 = ORIENTED_EDGE ( 'NONE', *, *, #6704, .F. ) ;
#9313 = CARTESIAN_POINT ( 'NONE',  ( -62.26794919243111082, 12.32366454968463110, 0.5000000000000013323 ) ) ;
#9314 = EDGE_CURVE ( 'NONE', #35, #3037, #1023, .T. ) ;
#9315 = VERTEX_POINT ( 'NONE', #1111 ) ;
#9316 = ORIENTED_EDGE ( 'NONE', *, *, #10276, .F. ) ;
#9317 = CARTESIAN_POINT ( 'NONE',  ( -61.13531646874998415, 8.890624999658601979, 1.500000000000002220 ) ) ;
#9318 = CARTESIAN_POINT ( 'NONE',  ( -62.49999999999998579, 15.91666666666666607, 2.366025403784441483 ) ) ;
#9319 = EDGE_CURVE ( 'NONE', #9377, #6183, #3661, .T. ) ;
#9320 = CARTESIAN_POINT ( 'NONE',  ( -62.86468353124998032, 13.74479166632526805, 1.000774730468978246 ) ) ;
#9321 = CARTESIAN_POINT ( 'NONE',  ( -60.99999999999998579, 8.218749999317202182, 1.500000000000002220 ) ) ;
#9322 = EDGE_LOOP ( 'NONE', ( #4036, #6244, #9597, #8639, #5325, #1092, #10480, #6413, #6175, #9685, #2484, #8926, #8753, #1357, #9796, #1828 ) ) ;
#9323 = PLANE ( 'NONE',  #547 ) ;
#9324 = ORIENTED_EDGE ( 'NONE', *, *, #1644, .F. ) ;
#9325 = FACE_OUTER_BOUND ( 'NONE', #8066, .T. ) ;
#9326 = CARTESIAN_POINT ( 'NONE',  ( -62.43234176562499016, 15.74479166632526628, 2.248837904296538071 ) ) ;
#9327 = CARTESIAN_POINT ( 'NONE',  ( -61.99999999999998579, 16.15624999931720041, 2.500000000000002665 ) ) ;
#9328 = DIRECTION ( 'NONE',  ( 0.9961946980917455452, 1.067350013832301058E-17, 0.08715574274765848506 ) ) ;
#9329 =( BOUNDED_CURVE ( )  B_SPLINE_CURVE ( 2, ( #5213, #4375, #3164, #6569, #2282, #6512, #10830, #8959, #6404 ),
 .UNSPECIFIED., .F., .T. ) 
 B_SPLINE_CURVE_WITH_KNOTS ( ( 3, 2, 2, 2, 3 ),
 ( 0.9453125000000000000, 0.9479166666666666297, 0.9531250000000000000, 0.9583333333333333703, 0.9609375000000000000 ),
 .UNSPECIFIED. ) 
 CURVE ( )  GEOMETRIC_REPRESENTATION_ITEM ( )  RATIONAL_B_SPLINE_CURVE ( ( 0.9330127018922194093, 0.9330127018922194093, 1.000000000000000000, 0.8660254037844387076, 1.000000000000000000, 0.8660254037844387076, 1.000000000000000000, 0.9330127018922194093, 0.9330127018922194093 ) ) 
 REPRESENTATION_ITEM ( '' )  );
#9330 = DIRECTION ( 'NONE',  ( 0.000000000000000000, 0.000000000000000000, -1.000000000000000000 ) ) ;
#9331 = CARTESIAN_POINT ( 'NONE',  ( -61.99999999999999289, 13.20312499965860198, 0.5015494609379544944 ) ) ;
#9332 = CARTESIAN_POINT ( 'NONE',  ( -61.13531646874998415, 8.348958332991935904, 1.000774730468978468 ) ) ;
#9333 = CYLINDRICAL_SURFACE ( 'NONE', #7790, 0.9999999999999981126 ) ;
#9334 = CARTESIAN_POINT ( 'NONE',  ( 145.0000000000000284, -5.500000000000000000, 6.000000000000000000 ) ) ;
#9335 = CARTESIAN_POINT ( 'NONE',  ( -62.43234176562499016, 9.307291666325268054, 2.248837904296538071 ) ) ;
#9336 = CARTESIAN_POINT ( 'NONE',  ( -61.99999999999998579, 14.18750000000000000, 2.500000000000002665 ) ) ;
#9337 = VERTEX_POINT ( 'NONE', #9726 ) ;
#9338 = LINE ( 'NONE', #4272, #9933 ) ;
#9339 = DIRECTION ( 'NONE',  ( -0.000000000000000000, -0.000000000000000000, 1.000000000000000000 ) ) ;
#9340 = EDGE_CURVE ( 'NONE', #8859, #3792, #4436, .T. ) ;
#9341 = CARTESIAN_POINT ( 'NONE',  ( -61.99999999999999289, 15.64062499965860198, 0.5015494609379544944 ) ) ;
#9342 = CARTESIAN_POINT ( 'NONE',  ( -61.99999999999998579, 11.51562499965860020, 2.498450539062049724 ) ) ;
#9343 = EDGE_CURVE ( 'NONE', #8297, #10242, #10076, .T. ) ;
#9344 = CARTESIAN_POINT ( 'NONE',  ( -62.86468353124999453, 15.28645833299193413, 1.999225269531025750 ) ) ;
#9345 = PLANE ( 'NONE',  #4980 ) ;
#9346 = ORIENTED_EDGE ( 'NONE', *, *, #2419, .F. ) ;
#9347 = CARTESIAN_POINT ( 'NONE',  ( -62.99999999999998579, 15.64583333333333393, 2.077350269189627952 ) ) ;
#9348 = CARTESIAN_POINT ( 'NONE',  ( -62.86468353124998032, 8.494791666325268054, 1.000774730468978024 ) ) ;
#9349 = CARTESIAN_POINT ( 'NONE',  ( -60.99999999999998579, 12.71874999931720396, 1.500000000000002220 ) ) ;
#9350 = CARTESIAN_POINT ( 'NONE',  ( 145.0000000000000284, -5.500000000000000000, 0.000000000000000000 ) ) ;
#9351 = LINE ( 'NONE', #853, #10513 ) ;
#9352 = AXIS2_PLACEMENT_3D ( 'NONE', #9876, #3930, #2992 ) ;
#9353 = CARTESIAN_POINT ( 'NONE',  ( -62.86468353124999453, 12.20312499965860198, 1.500000000000002220 ) ) ;
#9354 = CARTESIAN_POINT ( 'NONE',  ( -61.99999999999998579, 15.68749999999999645, 2.500000000000002665 ) ) ;
#9355 = VERTEX_POINT ( 'NONE', #7837 ) ;
#9356 = CARTESIAN_POINT ( 'NONE',  ( 146.0000000000000284, -5.500000000000000000, 3.000000000000000000 ) ) ;
#9357 = CARTESIAN_POINT ( 'NONE',  ( -61.99999999999998579, 12.82812499965860198, 2.498450539062049724 ) ) ;
#9358 = CARTESIAN_POINT ( 'NONE',  ( -61.99999999999998579, 11.40624999931720218, 2.500000000000002665 ) ) ;
#9359 = EDGE_CURVE ( 'NONE', #2994, #3747, #328, .T. ) ;
#9360 = MECHANICAL_DESIGN_GEOMETRIC_PRESENTATION_REPRESENTATION (  '', ( #8477 ), #3686 ) ;
#9361 = CARTESIAN_POINT ( 'NONE',  ( -61.49999999999998579, 9.677083332650534331, 2.366025403784441927 ) ) ;
#9362 = EDGE_LOOP ( 'NONE', ( #300, #9695, #8484, #5884 ) ) ;
#9363 = CARTESIAN_POINT ( 'NONE',  ( 0.000000000000000000, 0.000000000000000000, 0.000000000000000000 ) ) ;
#9364 = VECTOR ( 'NONE', #10817, 1000.000000000000000 ) ;
#9365 = ORIENTED_EDGE ( 'NONE', *, *, #3790, .F. ) ;
#9366 = CARTESIAN_POINT ( 'NONE',  ( -61.99999999999998579, 14.03124999931720218, 0.5000000000000013323 ) ) ;
#9367 = CARTESIAN_POINT ( 'NONE',  ( -61.13531646874998415, 11.57812499965860198, 1.500000000000002220 ) ) ;
#9368 = VECTOR ( 'NONE', #7727, 1000.000000000000000 ) ;
#9369 = ORIENTED_EDGE ( 'NONE', *, *, #6789, .F. ) ;
#9370 = VECTOR ( 'NONE', #4144, 1000.000000000000000 ) ;
#9371 = CARTESIAN_POINT ( 'NONE',  ( -61.99999999999998579, 9.328124999658600203, 2.498450539062049724 ) ) ;
#9372 = CARTESIAN_POINT ( 'NONE',  ( -49.99999999999998579, -4.000000000000019540, -2.000000000000000000 ) ) ;
#9373 = EDGE_CURVE ( 'NONE', #724, #292, #3335, .T. ) ;
#9374 = CIRCLE ( 'NONE', #4592, 1.099999999999989875 ) ;
#9375 = CARTESIAN_POINT ( 'NONE',  ( -62.86468353124998742, 12.53645833299193590, 1.999225269531025972 ) ) ;
#9376 = CARTESIAN_POINT ( 'NONE',  ( -61.49999999999998579, 13.29166666666666607, 0.6339745962155628467 ) ) ;
#9377 = VERTEX_POINT ( 'NONE', #2955 ) ;
#9378 = CYLINDRICAL_SURFACE ( 'NONE', #3906, 6.000000000000005329 ) ;
#9379 = ADVANCED_FACE ( 'NONE', ( #1167 ), #4546, .T. ) ;
#9380 = VERTEX_POINT ( 'NONE', #2062 ) ;
#9381 = CARTESIAN_POINT ( 'NONE',  ( -62.86468353124998032, 15.43229166632526805, 1.000774730468978246 ) ) ;
#9382 = VECTOR ( 'NONE', #6903, 1000.000000000000000 ) ;
#9383 = LINE ( 'NONE', #53, #8408 ) ;
#9384 = DIRECTION ( 'NONE',  ( 0.000000000000000000, 1.000000000000000000, 0.000000000000000000 ) ) ;
#9385 = FACE_OUTER_BOUND ( 'NONE', #3735, .T. ) ;
#9386 = CARTESIAN_POINT ( 'NONE',  ( -62.86468353124999453, 13.51562499965860020, 1.500000000000002220 ) ) ;
#9387 = CARTESIAN_POINT ( 'NONE',  ( -61.13531646874998415, 9.098958332991934128, 1.000774730468978468 ) ) ;
#9388 = CARTESIAN_POINT ( 'NONE',  ( 150.0000000000000284, -2.500000000000000444, 3.000000000000000000 ) ) ;
#9389 = LINE ( 'NONE', #7566, #6007 ) ;
#9390 = CARTESIAN_POINT ( 'NONE',  ( -61.13531646874998415, 8.661458332991935904, 1.000774730468978468 ) ) ;
#9391 = CARTESIAN_POINT ( 'NONE',  ( -60.99999999999998579, 15.69791666598386648, 2.077350269189628840 ) ) ;
#9392 = VERTEX_POINT ( 'NONE', #9671 ) ;
#9393 = CARTESIAN_POINT ( 'NONE',  ( -149.9999999999999716, -8.000000000000000000, 3.000000000000000000 ) ) ;
#9394 = CARTESIAN_POINT ( 'NONE',  ( -61.73205080756886076, 11.27008544963257286, 0.5000000000000044409 ) ) ;
#9395 = VECTOR ( 'NONE', #6941, 1000.000000000000000 ) ;
#9396 =( BOUNDED_CURVE ( )  B_SPLINE_CURVE ( 2, ( #7214, #2163, #317, #5596, #10421 ),
 .UNSPECIFIED., .F., .F. ) 
 B_SPLINE_CURVE_WITH_KNOTS ( ( 3, 2, 3 ),
 ( 0.9921875000000000000, 0.9947916666666666297, 1.000000000000000000 ),
 .UNSPECIFIED. ) 
 CURVE ( )  GEOMETRIC_REPRESENTATION_ITEM ( )  RATIONAL_B_SPLINE_CURVE ( ( 0.9330127018922194093, 0.9330127018922194093, 1.000000000000000000, 0.8660254037844387076, 1.000000000000000000 ) ) 
 REPRESENTATION_ITEM ( '' )  );
#9397 = CARTESIAN_POINT ( 'NONE',  ( -61.13531646874997705, 15.30729166632526983, 1.999225269531026417 ) ) ;
#9398 = CARTESIAN_POINT ( 'NONE',  ( -61.99999999999998579, 10.64062499965860376, 0.5015494609379544944 ) ) ;
#9399 = CARTESIAN_POINT ( 'NONE',  ( -61.13531646874997705, 8.807291666325268054, 1.999225269531026417 ) ) ;
#9400 = CARTESIAN_POINT ( 'NONE',  ( -61.73205080756886076, 9.770085449632574637, 0.5000000000000044409 ) ) ;
#9401 = ORIENTED_EDGE ( 'NONE', *, *, #7722, .F. ) ;
#9402 = CARTESIAN_POINT ( 'NONE',  ( -61.49999999999998579, 15.70833333333333037, 2.366025403784441927 ) ) ;
#9403 = CARTESIAN_POINT ( 'NONE',  ( -62.43234176562498305, 8.473958332991934128, 0.7511620957034662593 ) ) ;
#9404 = CARTESIAN_POINT ( 'NONE',  ( 0.000000000000000000, 0.000000000000000000, 0.000000000000000000 ) ) ;
#9405 = CARTESIAN_POINT ( 'NONE',  ( -61.49999999999998579, 13.42708333265053433, 2.366025403784441927 ) ) ;
#9406 = CARTESIAN_POINT ( 'NONE',  ( -61.99999999999998579, 14.93749999999999822, 2.500000000000002665 ) ) ;
#9407 = ORIENTED_EDGE ( 'NONE', *, *, #4221, .F. ) ;
#9408 = CARTESIAN_POINT ( 'NONE',  ( -61.49999999999998579, 9.791666666666667851, 0.6339745962155628467 ) ) ;
#9409 = EDGE_CURVE ( 'NONE', #9954, #302, #2898, .T. ) ;
#9410 = CARTESIAN_POINT ( 'NONE',  ( -62.43234176562499016, 11.49479166632526805, 2.248837904296538071 ) ) ;
#9411 = DIRECTION ( 'NONE',  ( 0.000000000000000000, -1.000000000000000000, 0.000000000000000000 ) ) ;
#9412 = DIRECTION ( 'NONE',  ( 0.000000000000000000, 0.000000000000000000, -1.000000000000000000 ) ) ;
#9413 = ORIENTED_EDGE ( 'NONE', *, *, #3094, .T. ) ;
#9414 = CARTESIAN_POINT ( 'NONE',  ( -61.99999999999998579, 15.43749999999999822, 2.500000000000002665 ) ) ;
#9415 = CARTESIAN_POINT ( 'NONE',  ( -61.13531646874998415, 12.61979166632526805, 1.999225269531026417 ) ) ;
#9416 = CARTESIAN_POINT ( 'NONE',  ( -61.99999999999998579, 12.06250000000000000, 0.5000000000000013323 ) ) ;
#9417 = CARTESIAN_POINT ( 'NONE',  ( -61.99999999999998579, 9.281249999317200405, 0.3452994616207497591 ) ) ;
#9418 = VERTEX_POINT ( 'NONE', #3608 ) ;
#9419 = CARTESIAN_POINT ( 'NONE',  ( -61.73205080756886076, 13.94866454968462932, 2.500000000000003109 ) ) ;
#9420 = EDGE_LOOP ( 'NONE', ( #3376, #282, #7947, #10761 ) ) ;
#9421 = CYLINDRICAL_SURFACE ( 'NONE', #1959, 0.9999999999999981126 ) ;
#9422 = CARTESIAN_POINT ( 'NONE',  ( -62.86468353124998032, 11.93229166632526628, 1.000774730468978246 ) ) ;
#9423 = EDGE_CURVE ( 'NONE', #8026, #3276, #9032, .T. ) ;
#9424 = SURFACE_STYLE_FILL_AREA ( #4419 ) ;
#9425 = ORIENTED_EDGE ( 'NONE', *, *, #3705, .T. ) ;
#9426 = VECTOR ( 'NONE', #2563, 1000.000000000000000 ) ;
#9427 = CARTESIAN_POINT ( 'NONE',  ( -62.43234176562499016, 8.807291666325268054, 2.248837904296538071 ) ) ;
#9428 = CARTESIAN_POINT ( 'NONE',  ( -62.49999999999998579, 15.83333333333333037, 0.6339745962155627357 ) ) ;
#9429 = CARTESIAN_POINT ( 'NONE',  ( -61.56765823437498852, 12.84895833299193413, 2.248837904296538515 ) ) ;
#9430 = CARTESIAN_POINT ( 'NONE',  ( -60.99999999999998579, 13.22916666666666607, 2.077350269189628840 ) ) ;
#9431 = ORIENTED_EDGE ( 'NONE', *, *, #10261, .F. ) ;
#9432 = AXIS2_PLACEMENT_3D ( 'NONE', #9791, #2184, #8961 ) ;
#9433 = LINE ( 'NONE', #100, #3197 ) ;
#9434 = ORIENTED_EDGE ( 'NONE', *, *, #3149, .T. ) ;
#9435 = CARTESIAN_POINT ( 'NONE',  ( -60.99999999999998579, 13.19791666598387003, 2.077350269189628840 ) ) ;
#9436 = CARTESIAN_POINT ( 'NONE',  ( -62.86468353124998032, 15.18229166632526805, 1.000774730468978246 ) ) ;
#9437 = CYLINDRICAL_SURFACE ( 'NONE', #2545, 0.9999999999999981126 ) ;
#9438 = DIRECTION ( 'NONE',  ( 0.000000000000000000, 0.000000000000000000, 1.000000000000000000 ) ) ;
#9439 = PLANE ( 'NONE',  #9021 ) ;
#9440 = CIRCLE ( 'NONE', #8570, 2.500000000000002220 ) ;
#9441 = CARTESIAN_POINT ( 'NONE',  ( -61.13531646874998415, 14.14062499965860198, 1.500000000000002220 ) ) ;
#9442 = AXIS2_PLACEMENT_3D ( 'NONE', #7225, #2115, #7001 ) ;
#9443 = CARTESIAN_POINT ( 'NONE',  ( -61.13531646874998415, 9.307291666325268054, 1.999225269531026417 ) ) ;
#9444 = DIRECTION ( 'NONE',  ( 0.000000000000000000, -1.000000000000000000, 0.000000000000000000 ) ) ;
#9445 = CARTESIAN_POINT ( 'NONE',  ( -139.9999999999999716, -43.00000000000000000, 0.000000000000000000 ) ) ;
#9446 = CARTESIAN_POINT ( 'NONE',  ( -61.99999999999998579, 8.953124999658601979, 0.5015494609379544944 ) ) ;
#9447 = FACE_OUTER_BOUND ( 'NONE', #3279, .T. ) ;
#9448 = ORIENTED_EDGE ( 'NONE', *, *, #5434, .F. ) ;
#9449 = LINE ( 'NONE', #8621, #4416 ) ;
#9450 = CARTESIAN_POINT ( 'NONE',  ( -61.99999999999998579, 11.31250000000000000, 0.5000000000000013323 ) ) ;
#9451 = AXIS2_PLACEMENT_3D ( 'NONE', #8239, #1455, #2288 ) ;
#9452 = CARTESIAN_POINT ( 'NONE',  ( -62.43234176562498305, 15.91145833299193590, 0.7511620957034662593 ) ) ;
#9453 = CARTESIAN_POINT ( 'NONE',  ( -62.43234176562499016, 10.99479166632526805, 2.248837904296538071 ) ) ;
#9454 = CARTESIAN_POINT ( 'NONE',  ( -61.13531646874998415, 8.328124999658601979, 1.500000000000002220 ) ) ;
#9455 = VERTEX_POINT ( 'NONE', #10499 ) ;
#9456 = CARTESIAN_POINT ( 'NONE',  ( -61.49999999999998579, 14.79166666666666607, 0.6339745962155628467 ) ) ;
#9457 = CARTESIAN_POINT ( 'NONE',  ( -62.43234176562499016, 10.30729166632526983, 2.248837904296538071 ) ) ;
#9458 =( REPRESENTATION_RELATIONSHIP ('NONE','NONE', #560, #8867 ) REPRESENTATION_RELATIONSHIP_WITH_TRANSFORMATION ( #3968 )SHAPE_REPRESENTATION_RELATIONSHIP( ) );
#9459 = CARTESIAN_POINT ( 'NONE',  ( 0.000000000000000000, 0.000000000000000000, 0.000000000000000000 ) ) ;
#9460 = VECTOR ( 'NONE', #6108, 1000.000000000000000 ) ;
#9461 = EDGE_CURVE ( 'NONE', #10821, #4361, #8072, .T. ) ;
#9462 = CARTESIAN_POINT ( 'NONE',  ( -62.49999999999998579, 13.80208333265053611, 0.6339745962155627357 ) ) ;
#9463 = CARTESIAN_POINT ( 'NONE',  ( -62.49999999999998579, 14.58333333333333393, 0.6339745962155627357 ) ) ;
#9464 = VERTEX_POINT ( 'NONE', #663 ) ;
#9465 = DIRECTION ( 'NONE',  ( -0.000000000000000000, -0.000000000000000000, 1.000000000000000000 ) ) ;
#9466 =( BOUNDED_CURVE ( )  B_SPLINE_CURVE ( 2, ( #6859, #10289, #7028, #10406, #2635, #2866, #7750, #5173, #6079 ),
 .UNSPECIFIED., .F., .T. ) 
 B_SPLINE_CURVE_WITH_KNOTS ( ( 3, 2, 2, 2, 3 ),
 ( 0.4453125000000000000, 0.4479166666666666852, 0.4531250000000000000, 0.4583333333333333148, 0.4609375000000000000 ),
 .UNSPECIFIED. ) 
 CURVE ( )  GEOMETRIC_REPRESENTATION_ITEM ( )  RATIONAL_B_SPLINE_CURVE ( ( 0.9330127018922194093, 0.9330127018922194093, 1.000000000000000000, 0.8660254037844387076, 1.000000000000000000, 0.8660254037844387076, 1.000000000000000000, 0.9330127018922194093, 0.9330127018922194093 ) ) 
 REPRESENTATION_ITEM ( '' )  );
#9467 = CARTESIAN_POINT ( 'NONE',  ( -62.86468353124998032, 11.18229166632526983, 1.000774730468978024 ) ) ;
#9468 = DIRECTION ( 'NONE',  ( 0.000000000000000000, 0.000000000000000000, -1.000000000000000000 ) ) ;
#9469 = LINE ( 'NONE', #6923, #7830 ) ;
#9470 = EDGE_LOOP ( 'NONE', ( #10124, #3887, #10824, #4096, #8962, #8847 ) ) ;
#9471 = CARTESIAN_POINT ( 'NONE',  ( -60.99999999999998579, 10.52083333333333393, 0.9226497308103762673 ) ) ;
#9472 = CARTESIAN_POINT ( 'NONE',  ( 0.000000000000000000, 0.000000000000000000, 0.000000000000000000 ) ) ;
#9473 = CARTESIAN_POINT ( 'NONE',  ( -61.99999999999998579, 14.20312499965860198, 0.5015494609379544944 ) ) ;
#9474 = CARTESIAN_POINT ( 'NONE',  ( -61.73205080756886076, 11.05133545031537068, 0.5000000000000014433 ) ) ;
#9475 = CARTESIAN_POINT ( 'NONE',  ( -60.99999999999998579, 9.218749999317203958, 1.500000000000002220 ) ) ;
#9476 = ORIENTED_EDGE ( 'NONE', *, *, #2693, .T. ) ;
#9477 = CARTESIAN_POINT ( 'NONE',  ( -61.99999999999998579, 14.06250000000000000, 0.5000000000000013323 ) ) ;
#9478 = CARTESIAN_POINT ( 'NONE',  ( -61.49999999999998579, 9.927083332650536107, 2.366025403784441927 ) ) ;
#9479 = CARTESIAN_POINT ( 'NONE',  ( -62.86468353124998032, 10.68229166632526628, 1.000774730468978246 ) ) ;
#9480 = ADVANCED_FACE ( 'NONE', ( #8179, #7394 ), #9111, .T. ) ;
#9481 = ORIENTED_EDGE ( 'NONE', *, *, #10968, .T. ) ;
#9482 = EDGE_CURVE ( 'NONE', #10003, #6970, #2176, .T. ) ;
#9483 = CARTESIAN_POINT ( 'NONE',  ( -62.43234176562498305, 8.973958332991934128, 0.7511620957034662593 ) ) ;
#9484 = EDGE_CURVE ( 'NONE', #7385, #3291, #719, .T. ) ;
#9485 = CARTESIAN_POINT ( 'NONE',  ( -61.99999999999998579, 14.32812499965860020, 2.498450539062049724 ) ) ;
#9486 = CARTESIAN_POINT ( 'NONE',  ( -61.73205080756886076, 13.19866454968462932, 2.500000000000003109 ) ) ;
#9487 = EDGE_LOOP ( 'NONE', ( #6758, #3563, #2915 ) ) ;
#9488 = LINE ( 'NONE', #2773, #10461 ) ;
#9489 = PRODUCT_RELATED_PRODUCT_CATEGORY ( 'part', '', ( #10959 ) ) ;
#9490 = ORIENTED_EDGE ( 'NONE', *, *, #4397, .F. ) ;
#9491 = CARTESIAN_POINT ( 'NONE',  ( -61.49999999999998579, 12.79166666666666607, 0.6339745962155628467 ) ) ;
#9492 = CARTESIAN_POINT ( 'NONE',  ( -62.99999999999998579, 8.875000000000001776, 1.500000000000001998 ) ) ;
#9493 = DIRECTION ( 'NONE',  ( 0.000000000000000000, 0.000000000000000000, 1.000000000000000000 ) ) ;
#9494 = LINE ( 'NONE', #8500, #4385 ) ;
#9495 = CARTESIAN_POINT ( 'NONE',  ( 11.30000000000000426, 0.000000000000000000, 0.000000000000000000 ) ) ;
#9496 = CARTESIAN_POINT ( 'NONE',  ( -61.56765823437498142, 13.43229166632526805, 0.7511620957034663704 ) ) ;
#9497 = CARTESIAN_POINT ( 'NONE',  ( -61.13531646874998415, 8.307291666325269830, 1.999225269531026417 ) ) ;
#9498 = DIRECTION ( 'NONE',  ( 1.110223024625156343E-15, 1.000000000000000000, -0.000000000000000000 ) ) ;
#9499 = DIRECTION ( 'NONE',  ( 0.000000000000000000, -0.000000000000000000, -1.000000000000000000 ) ) ;
#9500 = EDGE_CURVE ( 'NONE', #6298, #7493, #2178, .T. ) ;
#9501 = CARTESIAN_POINT ( 'NONE',  ( -61.13531646874998415, 11.16145833299193413, 1.000774730468978468 ) ) ;
#9502 = DIRECTION ( 'NONE',  ( -0.000000000000000000, -0.000000000000000000, -1.000000000000000000 ) ) ;
#9503 = ORIENTED_EDGE ( 'NONE', *, *, #9667, .T. ) ;
#9504 = DIRECTION ( 'NONE',  ( -1.000000000000000000, 0.000000000000000000, 0.000000000000000000 ) ) ;
#9505 = CARTESIAN_POINT ( 'NONE',  ( 150.0000000000000000, 2.500000000000000444, 3.000000000000000000 ) ) ;
#9506 = CARTESIAN_POINT ( 'NONE',  ( -61.99999999999998579, 16.00000000000000000, 2.500000000000000444 ) ) ;
#9507 = CARTESIAN_POINT ( 'NONE',  ( -62.86468353124998032, 12.93229166632526805, 1.000774730468978246 ) ) ;
#9508 = CARTESIAN_POINT ( 'NONE',  ( -61.13531646874997705, 8.348958332991934128, 1.000774730468978468 ) ) ;
#9509 = EDGE_CURVE ( 'NONE', #930, #10486, #2999, .T. ) ;
#9510 = FILL_AREA_STYLE ('',( #8517 ) ) ;
#9511 = ORIENTED_EDGE ( 'NONE', *, *, #1348, .F. ) ;
#9512 = CARTESIAN_POINT ( 'NONE',  ( -62.49999999999998579, 15.16666666666666607, 2.366025403784441483 ) ) ;
#9513 = CARTESIAN_POINT ( 'NONE',  ( -61.56765823437498852, 10.34895833299193413, 2.248837904296538515 ) ) ;
#9514 = CARTESIAN_POINT ( 'NONE',  ( -61.13531646874998415, 15.55729166632526628, 1.999225269531026417 ) ) ;
#9515 = CARTESIAN_POINT ( 'NONE',  ( -62.99999999999998579, 13.07291666598387003, 0.9226497308103756012 ) ) ;
#9516 = DIRECTION ( 'NONE',  ( -0.000000000000000000, -0.000000000000000000, 1.000000000000000000 ) ) ;
#9517 = ORIENTED_EDGE ( 'NONE', *, *, #4594, .T. ) ;
#9518 = ADVANCED_FACE ( 'NONE', ( #8957 ), #9949, .F. ) ;
#9519 = CARTESIAN_POINT ( 'NONE',  ( -60.99999999999998579, 9.729166666666667851, 2.077350269189628840 ) ) ;
#9520 = CARTESIAN_POINT ( 'NONE',  ( -61.13531646874997705, 11.05729166632526805, 1.999225269531026417 ) ) ;
#9521 = EDGE_CURVE ( 'NONE', #2251, #8495, #5583, .T. ) ;
#9522 = FACE_OUTER_BOUND ( 'NONE', #1505, .T. ) ;
#9523 = APPLICATION_CONTEXT ( 'automotive_design' ) ;
#9524 = CARTESIAN_POINT ( 'NONE',  ( -61.06765823437498852, 16.17968749948790119, 1.500000000000002220 ) ) ;
#9525 = ORIENTED_EDGE ( 'NONE', *, *, #6942, .T. ) ;
#9526 = CARTESIAN_POINT ( 'NONE',  ( -62.99999999999998579, 10.89583333333333393, 2.077350269189627952 ) ) ;
#9527 = DIRECTION ( 'NONE',  ( -0.000000000000000000, -1.000000000000000000, -0.000000000000000000 ) ) ;
#9528 = CARTESIAN_POINT ( 'NONE',  ( -61.13531646874998415, 13.64062499965860198, 1.500000000000002220 ) ) ;
#9529 = CARTESIAN_POINT ( 'NONE',  ( -61.99999999999998579, 10.18750000000000000, 2.500000000000002665 ) ) ;
#9530 = CARTESIAN_POINT ( 'NONE',  ( -62.49999999999998579, 9.635416665983870033, 2.366025403784441483 ) ) ;
#9531 = VERTEX_POINT ( 'NONE', #3114 ) ;
#9532 =( BOUNDED_CURVE ( )  B_SPLINE_CURVE ( 2, ( #8741, #288, #6299, #7069, #1358, #2134, #4724, #6240, #1240 ),
 .UNSPECIFIED., .F., .T. ) 
 B_SPLINE_CURVE_WITH_KNOTS ( ( 3, 2, 2, 2, 3 ),
 ( 0.2265625000000000000, 0.2291666666666666574, 0.2343750000000000000, 0.2395833333333333426, 0.2421874999999999722 ),
 .UNSPECIFIED. ) 
 CURVE ( )  GEOMETRIC_REPRESENTATION_ITEM ( )  RATIONAL_B_SPLINE_CURVE ( ( 0.9330127018922194093, 0.9330127018922194093, 1.000000000000000000, 0.8660254037844387076, 1.000000000000000000, 0.8660254037844387076, 1.000000000000000000, 0.9330127018922200755, 0.9330127018922194093 ) ) 
 REPRESENTATION_ITEM ( '' )  );
#9533 = CARTESIAN_POINT ( 'NONE',  ( -61.73205080756886076, 13.44866454968462932, 2.500000000000003109 ) ) ;
#9534 = PLANE ( 'NONE',  #10598 ) ;
#9535 = CARTESIAN_POINT ( 'NONE',  ( -62.86468353124998742, 11.72395833299193413, 1.999225269531025972 ) ) ;
#9536 =( NAMED_UNIT ( * ) SI_UNIT ( $, .STERADIAN. ) SOLID_ANGLE_UNIT ( ) );
#9537 = EDGE_LOOP ( 'NONE', ( #2894, #2438, #1787, #9503 ) ) ;
#9538 = AXIS2_PLACEMENT_3D ( 'NONE', #5732, #7462, #6632 ) ;
#9539 = CARTESIAN_POINT ( 'NONE',  ( -61.99999999999998579, 10.57812499965860198, 2.498450539062049724 ) ) ;
#9540 = DIRECTION ( 'NONE',  ( 1.000000000000000000, 0.000000000000000000, 0.000000000000000000 ) ) ;
#9541 = ADVANCED_FACE ( 'NONE', ( #4930 ), #3212, .T. ) ;
#9542 = CARTESIAN_POINT ( 'NONE',  ( -61.13531646874998415, 15.16145833299193590, 1.000774730468978468 ) ) ;
#9543 = CARTESIAN_POINT ( 'NONE',  ( -61.49999999999998579, 8.927083332650536107, 2.366025403784441927 ) ) ;
#9544 = ORIENTED_EDGE ( 'NONE', *, *, #8187, .F. ) ;
#9545 = CARTESIAN_POINT ( 'NONE',  ( -57.99999999999998579, 0.000000000000000000, 0.000000000000000000 ) ) ;
#9546 = CIRCLE ( 'NONE', #7265, 1.100000000000003642 ) ;
#9547 = ADVANCED_FACE ( 'NONE', ( #4716 ), #6619, .T. ) ;
#9548 = AXIS2_PLACEMENT_3D ( 'NONE', #10929, #10094, #7604 ) ;
#9549 = ORIENTED_EDGE ( 'NONE', *, *, #4412, .T. ) ;
#9550 = CARTESIAN_POINT ( 'NONE',  ( -61.99999999999998579, 16.00000000000000000, 0.5000000000000041078 ) ) ;
#9551 = CARTESIAN_POINT ( 'NONE',  ( -60.99999999999998579, 9.000000000000001776, 1.500000000000002220 ) ) ;
#9552 = CARTESIAN_POINT ( 'NONE',  ( -61.99999999999998579, 16.00000000000000000, 1.500000000000002220 ) ) ;
#9553 = CARTESIAN_POINT ( 'NONE',  ( -60.99999999999998579, 12.00000000000000000, 1.500000000000002220 ) ) ;
#9554 = DIRECTION ( 'NONE',  ( -0.000000000000000000, -0.000000000000000000, -1.000000000000000000 ) ) ;
#9555 = CARTESIAN_POINT ( 'NONE',  ( -61.56765823437498852, 13.84895833299193413, 2.248837904296538515 ) ) ;
#9556 = VECTOR ( 'NONE', #4498, 1000.000000000000000 ) ;
#9557 = CARTESIAN_POINT ( 'NONE',  ( -61.56765823437498142, 9.119791666325268054, 0.7511620957034663704 ) ) ;
#9558 = CARTESIAN_POINT ( 'NONE',  ( -61.99999999999998579, 16.00000000000000000, 0.5000000000000041078 ) ) ;
#9559 = CARTESIAN_POINT ( 'NONE',  ( -57.99999999999998579, 0.000000000000000000, 3.141811147483251965 ) ) ;
#9560 = CARTESIAN_POINT ( 'NONE',  ( -61.13531646874998415, 10.39062499965860198, 1.500000000000002220 ) ) ;
#9561 = AXIS2_PLACEMENT_3D ( 'NONE', #4582, #5296, #8765 ) ;
#9562 = CARTESIAN_POINT ( 'NONE',  ( -61.99999999999998579, 16.00000000000000000, 1.500000000000002220 ) ) ;
#9563 = ORIENTED_EDGE ( 'NONE', *, *, #6152, .T. ) ;
#9564 = CARTESIAN_POINT ( 'NONE',  ( -62.49999999999998579, 14.33333333333333393, 0.6339745962155627357 ) ) ;
#9565 = CARTESIAN_POINT ( 'NONE',  ( -60.99999999999998579, 11.21874999931720218, 1.500000000000002220 ) ) ;
#9566 = TOROIDAL_SURFACE ( 'NONE', #1763, 1.336466033005844434, 0.5999999999999999778 ) ;
#9567 = LINE ( 'NONE', #4505, #4127 ) ;
#9568 = EDGE_CURVE ( 'NONE', #10687, #1239, #5864, .T. ) ;
#9569 = CARTESIAN_POINT ( 'NONE',  ( -62.86468353124999453, 12.45312499965860198, 1.500000000000002220 ) ) ;
#9570 = CARTESIAN_POINT ( 'NONE',  ( -61.56765823437498142, 9.369791666325268054, 0.7511620957034663704 ) ) ;
#9571 = ORIENTED_EDGE ( 'NONE', *, *, #9639, .F. ) ;
#9572 = CARTESIAN_POINT ( 'NONE',  ( -61.99999999999998579, 15.81250000000000000, 0.3452994616207497591 ) ) ;
#9573 = CARTESIAN_POINT ( 'NONE',  ( -61.56765823437498852, 10.59895833299193413, 2.248837904296538515 ) ) ;
#9574 = CARTESIAN_POINT ( 'NONE',  ( -62.86468353124998742, 15.22395833299193590, 1.999225269531025972 ) ) ;
#9575 = CIRCLE ( 'NONE', #9049, 1.100000000000003642 ) ;
#9576 = CARTESIAN_POINT ( 'NONE',  ( -62.49999999999998579, 14.55208333265053611, 0.6339745962155627357 ) ) ;
#9577 = CARTESIAN_POINT ( 'NONE',  ( -120.0000000000000000, 3.999999999999980904, 0.000000000000000000 ) ) ;
#9578 = ORIENTED_EDGE ( 'NONE', *, *, #5180, .T. ) ;
#9579 = CARTESIAN_POINT ( 'NONE',  ( -76.99999999999998579, -11.50000000000000711, 8.000000000000000000 ) ) ;
#9580 =( GEOMETRIC_REPRESENTATION_CONTEXT ( 3 ) GLOBAL_UNCERTAINTY_ASSIGNED_CONTEXT ( ( #5491 ) ) GLOBAL_UNIT_ASSIGNED_CONTEXT ( ( #1967, #7858, #8522 ) ) REPRESENTATION_CONTEXT ( 'NONE', 'WORKASPACE' ) );
#9581 = CARTESIAN_POINT ( 'NONE',  ( -62.86468353124999453, 11.70312499965860198, 1.500000000000002220 ) ) ;
#9582 = CARTESIAN_POINT ( 'NONE',  ( -62.86468353124999453, 8.703124999658601979, 1.500000000000002220 ) ) ;
#9583 = CIRCLE ( 'NONE', #2482, 50.00000000000000000 ) ;
#9584 = DIRECTION ( 'NONE',  ( 0.000000000000000000, 0.000000000000000000, 1.000000000000000000 ) ) ;
#9585 = ORIENTED_EDGE ( 'NONE', *, *, #4800, .T. ) ;
#9586 = CARTESIAN_POINT ( 'NONE',  ( -61.49999999999998579, 11.79166666666666785, 0.6339745962155628467 ) ) ;
#9587 = FACE_OUTER_BOUND ( 'NONE', #71, .T. ) ;
#9588 = CARTESIAN_POINT ( 'NONE',  ( -61.56765823437498142, 14.43229166632526983, 0.7511620957034663704 ) ) ;
#9589 = FACE_OUTER_BOUND ( 'NONE', #2244, .T. ) ;
#9590 = CARTESIAN_POINT ( 'NONE',  ( -60.99999999999998579, 10.44791666598387003, 2.077350269189628840 ) ) ;
#9591 = ORIENTED_EDGE ( 'NONE', *, *, #10541, .T. ) ;
#9592 = EDGE_CURVE ( 'NONE', #869, #3127, #492, .T. ) ;
#9593 = LINE ( 'NONE', #2819, #9221 ) ;
#9594 = CARTESIAN_POINT ( 'NONE',  ( -120.0000000000000000, 15.67949192431120053, -2.000000000000000000 ) ) ;
#9595 = CARTESIAN_POINT ( 'NONE',  ( -61.13531646874998415, 10.82812499965860020, 1.500000000000002220 ) ) ;
#9596 = CARTESIAN_POINT ( 'NONE',  ( 0.3600944671415647891, -0.2500000000000000000, 1.887947737020718941 ) ) ;
#9597 = ORIENTED_EDGE ( 'NONE', *, *, #9894, .F. ) ;
#9598 = CARTESIAN_POINT ( 'NONE',  ( -62.86468353124999453, 10.26562499965860198, 1.500000000000002220 ) ) ;
#9599 = DIRECTION ( 'NONE',  ( 0.000000000000000000, 0.000000000000000000, 1.000000000000000000 ) ) ;
#9600 = EDGE_CURVE ( 'NONE', #947, #8873, #95, .T. ) ;
#9601 = CARTESIAN_POINT ( 'NONE',  ( -61.13531646874998415, 14.61979166632526805, 1.999225269531026417 ) ) ;
#9602 = CARTESIAN_POINT ( 'NONE',  ( -105.0000000000000000, -2.500000000000000000, 4.000000000000000000 ) ) ;
#9603 = EDGE_LOOP ( 'NONE', ( #7470, #2712, #2691, #5545 ) ) ;
#9604 = CARTESIAN_POINT ( 'NONE',  ( -62.49999999999998579, 9.416666666666666075, 2.366025403784441483 ) ) ;
#9605 = AXIS2_PLACEMENT_3D ( 'NONE', #10119, #2358, #5908 ) ;
#9606 = ORIENTED_EDGE ( 'NONE', *, *, #9213, .F. ) ;
#9607 = CARTESIAN_POINT ( 'NONE',  ( -61.99999999999998579, 8.812500000000000000, 0.5000000000000013323 ) ) ;
#9608 = CARTESIAN_POINT ( 'NONE',  ( -62.99999999999998579, 8.625000000000000000, 1.500000000000001998 ) ) ;
#9609 = DIRECTION ( 'NONE',  ( -0.000000000000000000, -1.000000000000000000, -0.000000000000000000 ) ) ;
#9610 = CARTESIAN_POINT ( 'NONE',  ( -61.06765823437498852, 16.03906249982930277, 1.500000000000002220 ) ) ;
#9611 = CARTESIAN_POINT ( 'NONE',  ( -60.99999999999998579, 10.73958333265053611, 0.9226497308103762673 ) ) ;
#9612 = CARTESIAN_POINT ( 'NONE',  ( -62.86468353124998032, 13.49479166632526805, 1.000774730468978024 ) ) ;
#9613 = CARTESIAN_POINT ( 'NONE',  ( -61.13531646874998415, 10.09895833299193413, 1.000774730468978468 ) ) ;
#9614 = UNCERTAINTY_MEASURE_WITH_UNIT (LENGTH_MEASURE( 1.000000000000000082E-05 ), #1804, 'distance_accuracy_value', 'NONE');
#9615 = EDGE_CURVE ( 'NONE', #6298, #3002, #3270, .T. ) ;
#9616 = LINE ( 'NONE', #6170, #6379 ) ;
#9617 = CARTESIAN_POINT ( 'NONE',  ( -62.99999999999998579, 9.604166666666667851, 0.9226497308103756012 ) ) ;
#9618 = ADVANCED_FACE ( 'NONE', ( #6878 ), #10881, .F. ) ;
#9619 = CARTESIAN_POINT ( 'NONE',  ( -61.99999999999998579, 10.07812499965860198, 2.498450539062049724 ) ) ;
#9620 = CARTESIAN_POINT ( 'NONE',  ( -61.99999999999998579, 16.00000000000000000, 0.5000000000000041078 ) ) ;
#9621 = VERTEX_POINT ( 'NONE', #5876 ) ;
#9622 = CARTESIAN_POINT ( 'NONE',  ( -1.101142831430589948E-16, -0.2499999999999997780, -1.455170506525537366 ) ) ;
#9623 = CARTESIAN_POINT ( 'NONE',  ( 143.9000000000000341, 5.500000000000000000, 6.000000000000000000 ) ) ;
#9624 = ORIENTED_EDGE ( 'NONE', *, *, #4304, .F. ) ;
#9625 = VECTOR ( 'NONE', #3117, 999.9999999999998863 ) ;
#9626 = DIRECTION ( 'NONE',  ( -0.000000000000000000, -1.000000000000000000, -0.000000000000000000 ) ) ;
#9627 = CARTESIAN_POINT ( 'NONE',  ( -61.13531646874998415, 13.07812499965860198, 1.500000000000002220 ) ) ;
#9628 = CARTESIAN_POINT ( 'NONE',  ( -62.43234176562498305, 9.411458332991935904, 0.7511620957034662593 ) ) ;
#9629 = CARTESIAN_POINT ( 'NONE',  ( 0.000000000000000000, 2.500000000000000000, 3.000000000000000000 ) ) ;
#9630 = EDGE_LOOP ( 'NONE', ( #9865, #4040, #4721, #7413 ) ) ;
#9631 = CARTESIAN_POINT ( 'NONE',  ( -61.99999999999998579, 8.406249999317203958, 2.500000000000003109 ) ) ;
#9632 = CARTESIAN_POINT ( 'NONE',  ( -62.86468353124999453, 10.28645833299193413, 1.999225269531025750 ) ) ;
#9633 = DIRECTION ( 'NONE',  ( -0.3420201433256693235, 0.9396926207859080948, 5.551115123125782702E-17 ) ) ;
#9634 = CARTESIAN_POINT ( 'NONE',  ( -62.43234176562498305, 15.91145833299193590, 0.7511620957034662593 ) ) ;
#9635 = CARTESIAN_POINT ( 'NONE',  ( -62.49999999999998579, 14.13541666598387003, 2.366025403784441483 ) ) ;
#9636 = DIRECTION ( 'NONE',  ( 0.000000000000000000, 0.000000000000000000, 1.000000000000000000 ) ) ;
#9637 = EDGE_LOOP ( 'NONE', ( #3046, #6918 ) ) ;
#9638 = AXIS2_PLACEMENT_3D ( 'NONE', #4395, #9640, #1014 ) ;
#9639 = EDGE_CURVE ( 'NONE', #5859, #7720, #10619, .T. ) ;
#9640 = DIRECTION ( 'NONE',  ( -0.000000000000000000, -1.000000000000000000, -0.000000000000000000 ) ) ;
#9641 = ORIENTED_EDGE ( 'NONE', *, *, #6084, .T. ) ;
#9642 = PRODUCT_RELATED_PRODUCT_CATEGORY ( 'part', '', ( #2270 ) ) ;
#9643 = CARTESIAN_POINT ( 'NONE',  ( -61.99999999999999289, 12.26562499965860198, 2.498450539062049724 ) ) ;
#9644 = CARTESIAN_POINT ( 'NONE',  ( -61.99999999999998579, 11.90624999931720041, 2.500000000000002665 ) ) ;
#9645 = LINE ( 'NONE', #8813, #7310 ) ;
#9646 = ORIENTED_EDGE ( 'NONE', *, *, #4359, .F. ) ;
#9647 = CARTESIAN_POINT ( 'NONE',  ( -62.99999999999998579, 12.64583333333333393, 2.077350269189627952 ) ) ;
#9648 = AXIS2_PLACEMENT_3D ( 'NONE', #9350, #8693, #10286 ) ;
#9649 = CARTESIAN_POINT ( 'NONE',  ( 0.5000000000000000000, -0.2500000000000001665, 1.911797424705720116 ) ) ;
#9650 = CARTESIAN_POINT ( 'NONE',  ( -61.13531646874998415, 13.91145833299193413, 1.000774730468978468 ) ) ;
#9651 = CARTESIAN_POINT ( 'NONE',  ( -61.99999999999998579, 14.93749999999999822, 2.500000000000002665 ) ) ;
#9652 = CARTESIAN_POINT ( 'NONE',  ( -61.49999999999998579, 10.92708333265053611, 2.366025403784441927 ) ) ;
#9653 = VERTEX_POINT ( 'NONE', #9372 ) ;
#9654 = CARTESIAN_POINT ( 'NONE',  ( -60.99999999999998579, 14.00000000000000000, 1.500000000000002220 ) ) ;
#9655 = CARTESIAN_POINT ( 'NONE',  ( -62.99999999999998579, 15.36458333265053611, 2.077350269189627952 ) ) ;
#9656 = CARTESIAN_POINT ( 'NONE',  ( -62.43234176562498305, 12.16145833299193413, 0.7511620957034662593 ) ) ;
#9657 = CARTESIAN_POINT ( 'NONE',  ( 0.000000000000000000, -0.2499999999999999445, 1.312875263449798879 ) ) ;
#9658 = VERTEX_POINT ( 'NONE', #1824 ) ;
#9659 = CARTESIAN_POINT ( 'NONE',  ( -62.86468353124998742, 9.786458332991934128, 1.999225269531025972 ) ) ;
#9660 = CARTESIAN_POINT ( 'NONE',  ( -61.99999999999998579, 15.65624999931720218, 2.500000000000002665 ) ) ;
#9661 = CARTESIAN_POINT ( 'NONE',  ( -62.43234176562499016, 14.55729166632526983, 2.248837904296538071 ) ) ;
#9662 = ORIENTED_EDGE ( 'NONE', *, *, #6711, .T. ) ;
#9663 = EDGE_CURVE ( 'NONE', #8255, #9464, #3113, .T. ) ;
#9664 = CARTESIAN_POINT ( 'NONE',  ( -61.99999999999998579, 16.00000000000000000, 1.500000000000002220 ) ) ;
#9665 = EDGE_LOOP ( 'NONE', ( #5132, #5633 ) ) ;
#9666 = CARTESIAN_POINT ( 'NONE',  ( -60.99999999999998579, 8.770833333333333925, 0.9226497308103762673 ) ) ;
#9667 = EDGE_CURVE ( 'NONE', #6433, #10637, #2456, .T. ) ;
#9668 = CARTESIAN_POINT ( 'NONE',  ( -62.99999999999998579, 8.645833333333333925, 2.077350269189627952 ) ) ;
#9669 = CARTESIAN_POINT ( 'NONE',  ( -78.99999999999998579, -11.50000000000000711, 8.000000000000000000 ) ) ;
#9670 = CARTESIAN_POINT ( 'NONE',  ( -78.99999999999998579, -11.50000000000000711, 8.000000000000000000 ) ) ;
#9671 = CARTESIAN_POINT ( 'NONE',  ( 146.0000000000000284, -5.500000000000000000, 0.000000000000000000 ) ) ;
#9672 = CARTESIAN_POINT ( 'NONE',  ( -61.56765823437498852, 14.84895833299193413, 2.248837904296538515 ) ) ;
#9673 = CARTESIAN_POINT ( 'NONE',  ( -62.43234176562498305, 9.661458332991934128, 0.7511620957034662593 ) ) ;
#9674 = LINE ( 'NONE', #10443, #150 ) ;
#9675 = CARTESIAN_POINT ( 'NONE',  ( 150.0000000000000000, -8.000000000000000000, 3.000000000000000000 ) ) ;
#9676 = CARTESIAN_POINT ( 'NONE',  ( -61.99999999999998579, 10.82812499965860198, 2.498450539062049724 ) ) ;
#9677 = CARTESIAN_POINT ( 'NONE',  ( -62.26794919243111082, 13.67633545031537068, 2.500000000000003109 ) ) ;
#9678 = ORIENTED_EDGE ( 'NONE', *, *, #175, .F. ) ;
#9679 = PLANE ( 'NONE',  #2840 ) ;
#9680 = CARTESIAN_POINT ( 'NONE',  ( -62.99999999999998579, 9.125000000000000000, 1.500000000000001998 ) ) ;
#9681 = VERTEX_POINT ( 'NONE', #6774 ) ;
#9682 = CARTESIAN_POINT ( 'NONE',  ( -62.86468353124998032, 12.43229166632526628, 1.000774730468978246 ) ) ;
#9683 = CARTESIAN_POINT ( 'NONE',  ( -61.99999999999999289, 10.64062499965860198, 0.5015494609379544944 ) ) ;
#9684 =( NAMED_UNIT ( * ) PLANE_ANGLE_UNIT ( ) SI_UNIT ( $, .RADIAN. ) );
#9685 = ORIENTED_EDGE ( 'NONE', *, *, #9844, .T. ) ;
#9686 = DIRECTION ( 'NONE',  ( 1.000000000000000000, 0.000000000000000000, 0.000000000000000000 ) ) ;
#9687 = CARTESIAN_POINT ( 'NONE',  ( -61.13531646874997705, 10.66145833299193413, 1.000774730468978468 ) ) ;
#9688 = PRODUCT_CONTEXT ( 'NONE', #4401, 'mechanical' ) ;
#9689 = CARTESIAN_POINT ( 'NONE',  ( -62.86468353124998032, 15.68229166632526628, 1.000774730468978246 ) ) ;
#9690 = CARTESIAN_POINT ( 'NONE',  ( -61.49999999999998579, 14.26041666598387003, 0.6339745962155628467 ) ) ;
#9691 = DIRECTION ( 'NONE',  ( -0.000000000000000000, -1.000000000000000000, -0.000000000000000000 ) ) ;
#9692 = ORIENTED_EDGE ( 'NONE', *, *, #508, .F. ) ;
#9693 = ADVANCED_FACE ( 'NONE', ( #1663 ), #3319, .T. ) ;
#9694 = PLANE ( 'NONE',  #1112 ) ;
#9695 = ORIENTED_EDGE ( 'NONE', *, *, #8073, .F. ) ;
#9696 = EDGE_CURVE ( 'NONE', #192, #1190, #2544, .T. ) ;
#9697 = CARTESIAN_POINT ( 'NONE',  ( -61.99999999999999289, 12.89062499965860198, 0.5015494609379544944 ) ) ;
#9698 = CARTESIAN_POINT ( 'NONE',  ( -61.99999999999998579, 8.140624999658601979, 0.5015494609379544944 ) ) ;
#9699 = CARTESIAN_POINT ( 'NONE',  ( 195.0000000000000000, -2.500000000000000000, 4.000000000000000000 ) ) ;
#9700 = VERTEX_POINT ( 'NONE', #1711 ) ;
#9701 = CARTESIAN_POINT ( 'NONE',  ( -61.49999999999998579, 12.79166666666666607, 0.6339745962155628467 ) ) ;
#9702 = FACE_OUTER_BOUND ( 'NONE', #10768, .T. ) ;
#9703 = CARTESIAN_POINT ( 'NONE',  ( -62.86468353124998032, 14.74479166632526628, 1.000774730468978246 ) ) ;
#9704 =( BOUNDED_CURVE ( )  B_SPLINE_CURVE ( 2, ( #5756, #6655, #3521, #8637, #4183, #4400, #3575, #5966, #9354 ),
 .UNSPECIFIED., .F., .F. ) 
 B_SPLINE_CURVE_WITH_KNOTS ( ( 3, 2, 2, 2, 3 ),
 ( 0.9453125000000000000, 0.9479166666666666297, 0.9531250000000000000, 0.9583333333333333703, 0.9609375000000000000 ),
 .UNSPECIFIED. ) 
 CURVE ( )  GEOMETRIC_REPRESENTATION_ITEM ( )  RATIONAL_B_SPLINE_CURVE ( ( 0.9330127018922194093, 0.9330127018922194093, 1.000000000000000000, 0.8660254037844387076, 1.000000000000000000, 0.8660254037844387076, 1.000000000000000000, 0.9330127018922194093, 0.9330127018922194093 ) ) 
 REPRESENTATION_ITEM ( '' )  );
#9705 = LINE ( 'NONE', #8934, #3890 ) ;
#9706 = CARTESIAN_POINT ( 'NONE',  ( -60.99999999999998579, 10.23958333265053788, 0.9226497308103762673 ) ) ;
#9707 = EDGE_LOOP ( 'NONE', ( #1751, #1162, #6722, #7267 ) ) ;
#9708 = CARTESIAN_POINT ( 'NONE',  ( 140.0000000000000284, -8.000000000000000000, 6.000000000000000000 ) ) ;
#9709 = LINE ( 'NONE', #5475, #5255 ) ;
#9710 = CARTESIAN_POINT ( 'NONE',  ( -62.43234176562498305, 12.66145833299193413, 0.7511620957034662593 ) ) ;
#9711 = ORIENTED_EDGE ( 'NONE', *, *, #4633, .T. ) ;
#9712 = EDGE_CURVE ( 'NONE', #312, #8261, #5366, .T. ) ;
#9713 = CARTESIAN_POINT ( 'NONE',  ( -61.13531646874998415, 9.890624999658601979, 1.500000000000002220 ) ) ;
#9714 = DIRECTION ( 'NONE',  ( 0.000000000000000000, 0.000000000000000000, 1.000000000000000000 ) ) ;
#9715 = CARTESIAN_POINT ( 'NONE',  ( -61.99999999999998579, 14.95312499965860198, 0.5015494609379544944 ) ) ;
#9716 = CARTESIAN_POINT ( 'NONE',  ( -61.99999999999998579, 14.68750000000000000, 2.500000000000002665 ) ) ;
#9717 = VERTEX_POINT ( 'NONE', #6218 ) ;
#9718 = DIRECTION ( 'NONE',  ( -0.000000000000000000, -1.000000000000000000, -0.000000000000000000 ) ) ;
#9719 = VECTOR ( 'NONE', #6548, 1000.000000000000000 ) ;
#9720 = ORIENTED_EDGE ( 'NONE', *, *, #4423, .F. ) ;
#9721 = CARTESIAN_POINT ( 'NONE',  ( -60.99999999999998579, 8.750000000000000000, 1.500000000000002220 ) ) ;
#9722 = CARTESIAN_POINT ( 'NONE',  ( -62.99999999999998579, 8.895833333333333925, 2.077350269189627952 ) ) ;
#9723 = DIRECTION ( 'NONE',  ( -0.000000000000000000, -1.000000000000000000, -0.000000000000000000 ) ) ;
#9724 = CARTESIAN_POINT ( 'NONE',  ( -61.49999999999998579, 12.04166666666666607, 0.6339745962155628467 ) ) ;
#9725 = ADVANCED_FACE ( 'NONE', ( #2886 ), #383, .T. ) ;
#9726 = CARTESIAN_POINT ( 'NONE',  ( -61.99999999999998579, 9.187500000000000000, 2.500000000000002665 ) ) ;
#9727 = CARTESIAN_POINT ( 'NONE',  ( -61.99999999999998579, 10.51562499965860198, 2.498450539062049724 ) ) ;
#9728 = CARTESIAN_POINT ( 'NONE',  ( -62.43234176562498305, 10.47395833299193413, 0.7511620957034662593 ) ) ;
#9729 = CARTESIAN_POINT ( 'NONE',  ( -62.26794919243111082, 12.07366454968463110, 0.5000000000000013323 ) ) ;
#9730 = ORIENTED_EDGE ( 'NONE', *, *, #4594, .F. ) ;
#9731 = CARTESIAN_POINT ( 'NONE',  ( -37.99999999999999289, -14.00000000000000888, 0.000000000000000000 ) ) ;
#9732 = ADVANCED_FACE ( 'NONE', ( #10312 ), #2714, .F. ) ;
#9733 = UNCERTAINTY_MEASURE_WITH_UNIT (LENGTH_MEASURE( 1.000000000000000082E-05 ), #5978, 'distance_accuracy_value', 'NONE');
#9734 = CARTESIAN_POINT ( 'NONE',  ( -62.99999999999998579, 9.145833333333333925, 2.077350269189627952 ) ) ;
#9735 = VECTOR ( 'NONE', #9843, 1000.000000000000000 ) ;
#9736 = VERTEX_POINT ( 'NONE', #4536 ) ;
#9737 = CARTESIAN_POINT ( 'NONE',  ( -62.26794919243111082, 10.29241454900183328, 0.5000000000000013323 ) ) ;
#9738 = CARTESIAN_POINT ( 'NONE',  ( -62.43234176562499016, 12.24479166632526805, 2.248837904296538071 ) ) ;
#9739 = VECTOR ( 'NONE', #831, 1000.000000000000000 ) ;
#9740 = CARTESIAN_POINT ( 'NONE',  ( -61.99999999999999289, 10.51562499965860198, 2.498450539062049724 ) ) ;
#9741 = CARTESIAN_POINT ( 'NONE',  ( -61.99999999999998579, 8.687500000000000000, 2.500000000000002665 ) ) ;
#9742 = ORIENTED_EDGE ( 'NONE', *, *, #8501, .F. ) ;
#9743 = CYLINDRICAL_SURFACE ( 'NONE', #2991, 1.000000000000000888 ) ;
#9744 = CARTESIAN_POINT ( 'NONE',  ( -61.99999999999999289, 11.57812499965860198, 2.498450539062049724 ) ) ;
#9745 = VECTOR ( 'NONE', #10503, 1000.000000000000000 ) ;
#9746 = SHAPE_DEFINITION_REPRESENTATION ( #3246, #8867 ) ;
#9747 = CARTESIAN_POINT ( 'NONE',  ( -61.13531646874998415, 14.84895833299193413, 1.000774730468978468 ) ) ;
#9748 = CARTESIAN_POINT ( 'NONE',  ( -61.49999999999998579, 15.26041666598387003, 0.6339745962155628467 ) ) ;
#9749 = CARTESIAN_POINT ( 'NONE',  ( -60.99999999999998579, 14.71874999931720218, 1.500000000000002220 ) ) ;
#9750 = EDGE_LOOP ( 'NONE', ( #7547, #9525, #1635, #4869, #9742, #6935, #8036, #1553 ) ) ;
#9751 = CARTESIAN_POINT ( 'NONE',  ( -61.73205080756886076, 16.02008544963257464, 0.5000000000000014433 ) ) ;
#9752 = VECTOR ( 'NONE', #4614, 1000.000000000000000 ) ;
#9753 = ORIENTED_EDGE ( 'NONE', *, *, #1614, .T. ) ;
#9754 =( GEOMETRIC_REPRESENTATION_CONTEXT ( 3 ) GLOBAL_UNCERTAINTY_ASSIGNED_CONTEXT ( ( #6410 ) ) GLOBAL_UNIT_ASSIGNED_CONTEXT ( ( #4346, #6927, #5239 ) ) REPRESENTATION_CONTEXT ( 'NONE', 'WORKASPACE' ) );
#9755 = CARTESIAN_POINT ( 'NONE',  ( -62.43234176562499016, 12.24479166632526805, 2.248837904296538071 ) ) ;
#9756 = CARTESIAN_POINT ( 'NONE',  ( -61.56765823437498142, 8.119791666325268054, 0.7511620957034663704 ) ) ;
#9757 = CARTESIAN_POINT ( 'NONE',  ( -61.99999999999997868, 10.53124999931720573, 0.5000000000000013323 ) ) ;
#9758 = EDGE_LOOP ( 'NONE', ( #6267, #9346, #6312, #3753 ) ) ;
#9759 = CARTESIAN_POINT ( 'NONE',  ( -61.99999999999998579, 12.93750000000000178, 2.654700538379254571 ) ) ;
#9760 = CARTESIAN_POINT ( 'NONE',  ( -60.99999999999998579, 9.020833333333333925, 0.9226497308103762673 ) ) ;
#9761 = AXIS2_PLACEMENT_3D ( 'NONE', #8647, #1816, #7157 ) ;
#9762 =( NAMED_UNIT ( * ) SI_UNIT ( $, .STERADIAN. ) SOLID_ANGLE_UNIT ( ) );
#9763 = CARTESIAN_POINT ( 'NONE',  ( -61.99999999999998579, 16.00000000000000000, 1.500000000000002220 ) ) ;
#9764 = CARTESIAN_POINT ( 'NONE',  ( -60.99999999999998579, 10.48958333265053611, 0.9226497308103762673 ) ) ;
#9765 = EDGE_CURVE ( 'NONE', #9717, #1119, #10547, .T. ) ;
#9766 =( GEOMETRIC_REPRESENTATION_CONTEXT ( 3 ) GLOBAL_UNCERTAINTY_ASSIGNED_CONTEXT ( ( #10707 ) ) GLOBAL_UNIT_ASSIGNED_CONTEXT ( ( #8264, #5017, #7425 ) ) REPRESENTATION_CONTEXT ( 'NONE', 'WORKASPACE' ) );
#9767 = EDGE_LOOP ( 'NONE', ( #2110, #8184 ) ) ;
#9768 = FACE_OUTER_BOUND ( 'NONE', #2185, .T. ) ;
#9769 = VECTOR ( 'NONE', #406, 1000.000000000000000 ) ;
#9770 = CARTESIAN_POINT ( 'NONE',  ( -62.86468353124999453, 13.20312499965860198, 1.500000000000002220 ) ) ;
#9771 = EDGE_CURVE ( 'NONE', #8454, #6686, #6887, .T. ) ;
#9772 = CARTESIAN_POINT ( 'NONE',  ( -61.56765823437498852, 8.598958332991934128, 2.248837904296538515 ) ) ;
#9773 =( BOUNDED_CURVE ( )  B_SPLINE_CURVE ( 2, ( #1986, #3763, #9478, #10306, #4415, #314, #5358, #202, #3701 ),
 .UNSPECIFIED., .F., .T. ) 
 B_SPLINE_CURVE_WITH_KNOTS ( ( 3, 2, 2, 2, 3 ),
 ( 0.2109375000000000000, 0.2135416666666666574, 0.2187500000000000000, 0.2239583333333333426, 0.2265625000000000000 ),
 .UNSPECIFIED. ) 
 CURVE ( )  GEOMETRIC_REPRESENTATION_ITEM ( )  RATIONAL_B_SPLINE_CURVE ( ( 0.9330127018922194093, 0.9330127018922194093, 1.000000000000000000, 0.8660254037844387076, 1.000000000000000000, 0.8660254037844387076, 1.000000000000000000, 0.9330127018922194093, 0.9330127018922194093 ) ) 
 REPRESENTATION_ITEM ( '' )  );
#9774 = EDGE_LOOP ( 'NONE', ( #7273, #9851, #2826, #7891 ) ) ;
#9775 = CARTESIAN_POINT ( 'NONE',  ( -62.86468353124998032, 10.49479166632526983, 1.000774730468978246 ) ) ;
#9776 = DIRECTION ( 'NONE',  ( 0.000000000000000000, 1.000000000000000000, 0.000000000000000000 ) ) ;
#9777 = CARTESIAN_POINT ( 'NONE',  ( -62.86468353124998032, 15.74479166632526805, 1.000774730468978246 ) ) ;
#9778 = LINE ( 'NONE', #8893, #4826 ) ;
#9779 = VERTEX_POINT ( 'NONE', #3537 ) ;
#9780 = CYLINDRICAL_SURFACE ( 'NONE', #10469, 0.9999999999999981126 ) ;
#9781 = EDGE_CURVE ( 'NONE', #5253, #4602, #9931, .T. ) ;
#9782 = ORIENTED_EDGE ( 'NONE', *, *, #4892, .T. ) ;
#9783 = CARTESIAN_POINT ( 'NONE',  ( -49.99999999999998579, 2.500000000000000000, 3.000000000000000000 ) ) ;
#9784 = CARTESIAN_POINT ( 'NONE',  ( -62.99999999999998579, 9.145833333333333925, 2.077350269189627952 ) ) ;
#9785 = CARTESIAN_POINT ( 'NONE',  ( -42.47213595499957961, -10.00000000000000888, 3.000000000000000000 ) ) ;
#9786 = CARTESIAN_POINT ( 'NONE',  ( -61.73205080756886076, 12.05133545031537068, 0.5000000000000014433 ) ) ;
#9787 = CARTESIAN_POINT ( 'NONE',  ( -61.49999999999998579, 8.291666666666666075, 0.6339745962155628467 ) ) ;
#9788 = CARTESIAN_POINT ( 'NONE',  ( -61.99999999999998579, 10.14062499965860198, 0.5015494609379544944 ) ) ;
#9789 = CARTESIAN_POINT ( 'NONE',  ( -61.49999999999998579, 15.42708333265053611, 2.366025403784441927 ) ) ;
#9790 = CARTESIAN_POINT ( 'NONE',  ( -62.43234176562499016, 12.05729166632526628, 2.248837904296538071 ) ) ;
#9791 = CARTESIAN_POINT ( 'NONE',  ( 0.5000000000000000000, 0.000000000000000000, 0.000000000000000000 ) ) ;
#9792 = ORIENTED_EDGE ( 'NONE', *, *, #10358, .T. ) ;
#9793 = VECTOR ( 'NONE', #5587, 1000.000000000000000 ) ;
#9794 = CARTESIAN_POINT ( 'NONE',  ( -37.99999999999999289, -14.00000000000000888, 0.000000000000000000 ) ) ;
#9795 = DIRECTION ( 'NONE',  ( 0.000000000000000000, 0.000000000000000000, -1.000000000000000000 ) ) ;
#9796 = ORIENTED_EDGE ( 'NONE', *, *, #10843, .F. ) ;
#9797 = CARTESIAN_POINT ( 'NONE',  ( -62.99999999999998579, 10.32291666598387003, 0.9226497308103756012 ) ) ;
#9798 = CARTESIAN_POINT ( 'NONE',  ( -61.56765823437498142, 14.11979166632526805, 0.7511620957034663704 ) ) ;
#9799 = CARTESIAN_POINT ( 'NONE',  ( -61.13531646874998415, 10.07812499965860198, 1.500000000000002220 ) ) ;
#9800 = PLANE ( 'NONE',  #3518 ) ;
#9801 = EDGE_LOOP ( 'NONE', ( #3862, #9880, #3041, #1493 ) ) ;
#9802 = CARTESIAN_POINT ( 'NONE',  ( 0.5000000000000000000, 0.000000000000000000, 1.928074011315806136 ) ) ;
#9803 = CARTESIAN_POINT ( 'NONE',  ( -62.86468353124998032, 11.24479166632526805, 1.000774730468978024 ) ) ;
#9804 = CARTESIAN_POINT ( 'NONE',  ( -49.99998799999998766, 0.000000000000000000, 3.141811147483251965 ) ) ;
#9805 = CARTESIAN_POINT ( 'NONE',  ( -60.99999999999998579, 13.98958333265053788, 0.9226497308103762673 ) ) ;
#9806 = DIRECTION ( 'NONE',  ( 1.000000000000000000, -0.000000000000000000, 0.000000000000000000 ) ) ;
#9807 = EDGE_LOOP ( 'NONE', ( #4083, #2171, #7244, #2865 ) ) ;
#9808 = ORIENTED_EDGE ( 'NONE', *, *, #2266, .T. ) ;
#9809 = VECTOR ( 'NONE', #4003, 1000.000000000000000 ) ;
#9810 = TOROIDAL_SURFACE ( 'NONE', #38, 1.336466033005844434, 0.5999999999999999778 ) ;
#9811 = CARTESIAN_POINT ( 'NONE',  ( -61.13531646874997705, 13.09895833299193413, 1.000774730468978468 ) ) ;
#9812 = CARTESIAN_POINT ( 'NONE',  ( -62.86468353124998742, 8.473958332991934128, 1.999225269531025972 ) ) ;
#9813 = CARTESIAN_POINT ( 'NONE',  ( -62.49999999999998579, 8.416666666666666075, 2.366025403784441483 ) ) ;
#9814 = VERTEX_POINT ( 'NONE', #7888 ) ;
#9815 = CARTESIAN_POINT ( 'NONE',  ( -62.99999999999998579, 11.85416666666666607, 0.9226497308103756012 ) ) ;
#9816 = ADVANCED_FACE ( 'NONE', ( #1881 ), #7108, .F. ) ;
#9817 = PLANE ( 'NONE',  #5893 ) ;
#9818 =( NAMED_UNIT ( * ) SI_UNIT ( $, .STERADIAN. ) SOLID_ANGLE_UNIT ( ) );
#9819 = CARTESIAN_POINT ( 'NONE',  ( 0.5477065543514035850, 0.000000000000000000, 0.000000000000000000 ) ) ;
#9820 = AXIS2_PLACEMENT_3D ( 'NONE', #8469, #6755, #4909 ) ;
#9821 = CARTESIAN_POINT ( 'NONE',  ( -62.99999999999998579, 10.07291666598387003, 0.9226497308103756012 ) ) ;
#9822 = ORIENTED_EDGE ( 'NONE', *, *, #9771, .T. ) ;
#9823 = CARTESIAN_POINT ( 'NONE',  ( -62.26794919243111082, 13.42633545031536890, 2.500000000000003109 ) ) ;
#9824 = CIRCLE ( 'NONE', #7692, 1.934182851860891672 ) ;
#9825 = CARTESIAN_POINT ( 'NONE',  ( -61.56765823437498142, 12.86979166632526805, 0.7511620957034663704 ) ) ;
#9826 = CARTESIAN_POINT ( 'NONE',  ( -99.99999999999995737, -12.99999999999998757, 3.000000000000000000 ) ) ;
#9827 = VERTEX_POINT ( 'NONE', #10488 ) ;
#9828 = CARTESIAN_POINT ( 'NONE',  ( -61.56765823437498142, 11.93229166632526805, 0.7511620957034663704 ) ) ;
#9829 = CYLINDRICAL_SURFACE ( 'NONE', #7610, 0.9999999999999981126 ) ;
#9830 = VECTOR ( 'NONE', #4822, 1000.000000000000000 ) ;
#9831 = CARTESIAN_POINT ( 'NONE',  ( -61.99999999999998579, 15.32812499965860198, 2.498450539062049724 ) ) ;
#9832 = B_SPLINE_CURVE_WITH_KNOTS ( 'NONE', 3,
 ( #10333, #946, #5267, #1844, #4325, #1897 ),
 .UNSPECIFIED., .F., .F.,
 ( 4, 2, 4 ),
 ( 0.003191392849877886309, 0.003612977948258624256, 0.004034563046639362202 ),
 .UNSPECIFIED. ) ;
#9833 = ORIENTED_EDGE ( 'NONE', *, *, #3927, .T. ) ;
#9834 = DIRECTION ( 'NONE',  ( 0.000000000000000000, 0.000000000000000000, -1.000000000000000000 ) ) ;
#9835 = EDGE_CURVE ( 'NONE', #8026, #724, #7940, .T. ) ;
#9836 =( BOUNDED_CURVE ( )  B_SPLINE_CURVE ( 2, ( #4328, #4273, #7683, #2618, #4445, #286, #7847, #5327, #232 ),
 .UNSPECIFIED., .F., .T. ) 
 B_SPLINE_CURVE_WITH_KNOTS ( ( 3, 2, 2, 2, 3 ),
 ( 0.5859375000000000000, 0.5885416666666666297, 0.5937500000000000000, 0.5989583333333333703, 0.6015625000000000000 ),
 .UNSPECIFIED. ) 
 CURVE ( )  GEOMETRIC_REPRESENTATION_ITEM ( )  RATIONAL_B_SPLINE_CURVE ( ( 0.9330127018922194093, 0.9330127018922194093, 1.000000000000000000, 0.8660254037844387076, 1.000000000000000000, 0.8660254037844387076, 1.000000000000000000, 0.9330127018922194093, 0.9330127018922194093 ) ) 
 REPRESENTATION_ITEM ( '' )  );
#9837 = EDGE_CURVE ( 'NONE', #9380, #9377, #5249, .T. ) ;
#9838 = ORIENTED_EDGE ( 'NONE', *, *, #2487, .F. ) ;
#9839 = CARTESIAN_POINT ( 'NONE',  ( -61.99999999999998579, 9.531249999317202182, 0.5000000000000013323 ) ) ;
#9840 = CARTESIAN_POINT ( 'NONE',  ( -60.99999999999998579, 9.520833333333333925, 0.9226497308103762673 ) ) ;
#9841 = CARTESIAN_POINT ( 'NONE',  ( -139.9999999999999716, -8.000000000000000000, 3.000000000000000000 ) ) ;
#9842 = CYLINDRICAL_SURFACE ( 'NONE', #10963, 0.9999999999999981126 ) ;
#9843 = DIRECTION ( 'NONE',  ( -1.000000000000000000, -0.000000000000000000, -0.000000000000000000 ) ) ;
#9844 = EDGE_CURVE ( 'NONE', #211, #9653, #4596, .T. ) ;
#9845 = CARTESIAN_POINT ( 'NONE',  ( -61.99999999999998579, 16.00000000000000000, 1.500000000000002220 ) ) ;
#9846 = CARTESIAN_POINT ( 'NONE',  ( -62.43234176562498305, 12.47395833299193413, 0.7511620957034662593 ) ) ;
#9847 = CARTESIAN_POINT ( 'NONE',  ( -62.26794919243111082, 12.04241454900183328, 0.5000000000000013323 ) ) ;
#9848 = ORIENTED_EDGE ( 'NONE', *, *, #7584, .T. ) ;
#9849 = CARTESIAN_POINT ( 'NONE',  ( -120.0000000000000000, 14.99999999999998579, -2.000000000000000000 ) ) ;
#9850 = CARTESIAN_POINT ( 'NONE',  ( -60.99999999999998579, 15.22916666666666607, 2.077350269189628840 ) ) ;
#9851 = ORIENTED_EDGE ( 'NONE', *, *, #8536, .F. ) ;
#9852 = CARTESIAN_POINT ( 'NONE',  ( -60.99999999999998579, 13.73958333265053611, 0.9226497308103762673 ) ) ;
#9853 = CARTESIAN_POINT ( 'NONE',  ( -61.13531646874998415, 14.09895833299193413, 1.000774730468978468 ) ) ;
#9854 = CARTESIAN_POINT ( 'NONE',  ( -61.99999999999999289, 10.39062499965860198, 0.5015494609379544944 ) ) ;
#9855 = CARTESIAN_POINT ( 'NONE',  ( -77.99999999999998579, 11.49999999999999645, 8.000000000000000000 ) ) ;
#9856 = EDGE_LOOP ( 'NONE', ( #2214, #9034, #6781, #2803 ) ) ;
#9857 = FACE_OUTER_BOUND ( 'NONE', #10663, .T. ) ;
#9858 = CARTESIAN_POINT ( 'NONE',  ( -61.13531646874997705, 11.91145833299193413, 1.000774730468978468 ) ) ;
#9859 = EDGE_CURVE ( 'NONE', #6336, #10601, #208, .T. ) ;
#9860 = CARTESIAN_POINT ( 'NONE',  ( -77.99999999999998579, -11.50000000000000711, -3.300000000000004263 ) ) ;
#9861 = CARTESIAN_POINT ( 'NONE',  ( -61.99999999999998579, 16.00000000000000000, 1.500000000000002220 ) ) ;
#9862 = CARTESIAN_POINT ( 'NONE',  ( -62.99999999999998579, 15.57291666598387003, 0.9226497308103756012 ) ) ;
#9863 = ORIENTED_EDGE ( 'NONE', *, *, #6322, .F. ) ;
#9864 = CARTESIAN_POINT ( 'NONE',  ( -120.0000000000000000, 14.99999999999998579, 83.15773105863907233 ) ) ;
#9865 = ORIENTED_EDGE ( 'NONE', *, *, #4832, .F. ) ;
#9866 = EDGE_CURVE ( 'NONE', #2471, #2202, #8659, .T. ) ;
#9867 = CARTESIAN_POINT ( 'NONE',  ( -62.86468353124999453, 13.97395833299193413, 1.999225269531025750 ) ) ;
#9868 = CARTESIAN_POINT ( 'NONE',  ( -61.56765823437498852, 9.786458332991934128, 2.248837904296538515 ) ) ;
#9869 = CARTESIAN_POINT ( 'NONE',  ( -62.26794919243111082, 8.426335450315370679, 2.500000000000001776 ) ) ;
#9870 = ORIENTED_EDGE ( 'NONE', *, *, #10917, .F. ) ;
#9871 = CARTESIAN_POINT ( 'NONE',  ( -62.99999999999998579, 13.89583333333333393, 2.077350269189627952 ) ) ;
#9872 = DIRECTION ( 'NONE',  ( -0.000000000000000000, -1.000000000000000000, -0.000000000000000000 ) ) ;
#9873 = ADVANCED_FACE ( 'NONE', ( #1275 ), #152, .F. ) ;
#9874 = SURFACE_STYLE_FILL_AREA ( #7317 ) ;
#9875 = CARTESIAN_POINT ( 'NONE',  ( -62.49999999999998579, 11.88541666598387003, 2.366025403784441483 ) ) ;
#9876 = CARTESIAN_POINT ( 'NONE',  ( -139.9999999999999716, -8.000000000000000000, 3.000000000000000000 ) ) ;
#9877 = EDGE_CURVE ( 'NONE', #1578, #1253, #144, .T. ) ;
#9878 = CARTESIAN_POINT ( 'NONE',  ( -61.56765823437498142, 13.11979166632526805, 0.7511620957034663704 ) ) ;
#9879 = CARTESIAN_POINT ( 'NONE',  ( 0.5000000000000000000, 0.2499999999999998335, 2.000000000000000000 ) ) ;
#9880 = ORIENTED_EDGE ( 'NONE', *, *, #7451, .T. ) ;
#9881 = CARTESIAN_POINT ( 'NONE',  ( -61.13531646874998415, 11.39062499965860020, 1.500000000000002220 ) ) ;
#9882 = CARTESIAN_POINT ( 'NONE',  ( -144.9999999999999432, 8.000000000000000000, 3.000000000000000000 ) ) ;
#9883 = CARTESIAN_POINT ( 'NONE',  ( -61.99999999999998579, 15.45312499965860020, 0.5015494609379544944 ) ) ;
#9884 = ORIENTED_EDGE ( 'NONE', *, *, #10767, .F. ) ;
#9885 = CARTESIAN_POINT ( 'NONE',  ( -61.99999999999998579, -15.00000000000001421, 0.5000000000000013323 ) ) ;
#9886 = ORIENTED_EDGE ( 'NONE', *, *, #2096, .T. ) ;
#9887 = LINE ( 'NONE', #1391, #224 ) ;
#9888 = CARTESIAN_POINT ( 'NONE',  ( -60.99999999999998579, 10.02083333333333215, 0.9226497308103762673 ) ) ;
#9889 = CARTESIAN_POINT ( 'NONE',  ( -61.99999999999998579, 16.00000000000000000, 0.5000000000000041078 ) ) ;
#9890 = CARTESIAN_POINT ( 'NONE',  ( -61.73205080756886787, 8.448664549684631098, 2.500000000000004885 ) ) ;
#9891 = DIRECTION ( 'NONE',  ( 0.000000000000000000, 0.000000000000000000, -1.000000000000000000 ) ) ;
#9892 = CARTESIAN_POINT ( 'NONE',  ( -62.99999999999998579, 8.572916665983868256, 0.9226497308103756012 ) ) ;
#9893 = CARTESIAN_POINT ( 'NONE',  ( -61.99999999999998579, 11.57812499965860198, 2.498450539062049724 ) ) ;
#9894 = EDGE_CURVE ( 'NONE', #4539, #7385, #10426, .T. ) ;
#9895 = CARTESIAN_POINT ( 'NONE',  ( -114.9999999999999147, -43.00000000000000000, 0.000000000000000000 ) ) ;
#9896 = ORIENTED_EDGE ( 'NONE', *, *, #8228, .F. ) ;
#9897 = CARTESIAN_POINT ( 'NONE',  ( -61.99999999999998579, 15.43749999999999822, 2.500000000000002665 ) ) ;
#9898 = CARTESIAN_POINT ( 'NONE',  ( 0.5000000000000000000, 0.2499999999999998335, 1.911797424705720116 ) ) ;
#9899 = AXIS2_PLACEMENT_3D ( 'NONE', #8108, #3878, #7269 ) ;
#9900 = PRODUCT_DEFINITION_SHAPE ( 'NONE', 'NONE',  #10984 ) ;
#9901 = ORIENTED_EDGE ( 'NONE', *, *, #3305, .T. ) ;
#9902 = LINE ( 'NONE', #1459, #1474 ) ;
#9903 = CARTESIAN_POINT ( 'NONE',  ( -62.43234176562498305, 14.41145833299193413, 0.7511620957034662593 ) ) ;
#9904 = CARTESIAN_POINT ( 'NONE',  ( -62.86468353124999453, 9.953124999658601979, 1.500000000000002220 ) ) ;
#9905 = CARTESIAN_POINT ( 'NONE',  ( -61.99999999999998579, 14.43749999999999822, 2.500000000000002665 ) ) ;
#9906 = VERTEX_POINT ( 'NONE', #8776 ) ;
#9907 = CARTESIAN_POINT ( 'NONE',  ( -61.99999999999998579, 8.406249999317203958, 2.500000000000003109 ) ) ;
#9908 = CARTESIAN_POINT ( 'NONE',  ( -61.99999999999999289, 11.70312499965860198, 0.5015494609379544944 ) ) ;
#9909 = VECTOR ( 'NONE', #7752, 1000.000000000000000 ) ;
#9910 = CARTESIAN_POINT ( 'NONE',  ( -61.13531646874998415, 15.61979166632526628, 1.999225269531026417 ) ) ;
#9911 = ITEM_DEFINED_TRANSFORMATION ( 'NONE', 'NONE', #7809,  #2307 ) ;
#9912 = CARTESIAN_POINT ( 'NONE',  ( -61.99999999999998579, 15.18750000000000000, 2.500000000000002665 ) ) ;
#9913 = CARTESIAN_POINT ( 'NONE',  ( -62.49999999999998579, 16.13541666598386826, 2.366025403784441483 ) ) ;
#9914 = LINE ( 'NONE', #10848, #2343 ) ;
#9915 = EDGE_LOOP ( 'NONE', ( #4107, #8599, #7144, #2890 ) ) ;
#9916 = CARTESIAN_POINT ( 'NONE',  ( -62.49999999999998579, 11.88541666598387003, 2.366025403784441483 ) ) ;
#9917 = CARTESIAN_POINT ( 'NONE',  ( -120.0000000000000000, 3.999999999999980904, 0.000000000000000000 ) ) ;
#9918 = EDGE_CURVE ( 'NONE', #1268, #1104, #2269, .T. ) ;
#9919 = AXIS2_PLACEMENT_3D ( 'NONE', #6051, #3382, #9438 ) ;
#9920 = CARTESIAN_POINT ( 'NONE',  ( -61.13531646874998415, 14.82812499965860020, 1.500000000000002220 ) ) ;
#9921 = CARTESIAN_POINT ( 'NONE',  ( -62.86468353124999453, 9.453124999658600203, 1.500000000000002220 ) ) ;
#9922 = AXIS2_PLACEMENT_3D ( 'NONE', #2779, #221, #6340 ) ;
#9923 = DIRECTION ( 'NONE',  ( -0.000000000000000000, -1.000000000000000000, -0.000000000000000000 ) ) ;
#9924 = ORIENTED_EDGE ( 'NONE', *, *, #4446, .F. ) ;
#9925 = CARTESIAN_POINT ( 'NONE',  ( -62.99999999999998579, 13.87500000000000000, 1.500000000000001998 ) ) ;
#9926 = CARTESIAN_POINT ( 'NONE',  ( -62.49999999999998579, 8.635416665983868256, 2.366025403784441483 ) ) ;
#9927 =( LENGTH_UNIT ( ) NAMED_UNIT ( * ) SI_UNIT ( .MILLI., .METRE. ) );
#9928 = AXIS2_PLACEMENT_3D ( 'NONE', #7009, #2067, #9499 ) ;
#9929 = CARTESIAN_POINT ( 'NONE',  ( -62.99999999999998579, 11.86458333265053611, 2.077350269189627952 ) ) ;
#9930 = VECTOR ( 'NONE', #2935, 1000.000000000000000 ) ;
#9931 =( BOUNDED_CURVE ( )  B_SPLINE_CURVE ( 2, ( #1095, #1035, #1213, #7046, #7825, #4482, #3770, #2106, #9660 ),
 .UNSPECIFIED., .F., .F. ) 
 B_SPLINE_CURVE_WITH_KNOTS ( ( 3, 2, 2, 2, 3 ),
 ( 0.9140625000000000000, 0.9166666666666666297, 0.9218750000000000000, 0.9270833333333333703, 0.9296875000000000000 ),
 .UNSPECIFIED. ) 
 CURVE ( )  GEOMETRIC_REPRESENTATION_ITEM ( )  RATIONAL_B_SPLINE_CURVE ( ( 0.9330127018922194093, 0.9330127018922194093, 1.000000000000000000, 0.8660254037844387076, 1.000000000000000000, 0.8660254037844387076, 1.000000000000000000, 0.9330127018922194093, 0.9330127018922194093 ) ) 
 REPRESENTATION_ITEM ( '' )  );
#9932 = CARTESIAN_POINT ( 'NONE',  ( -61.56765823437498852, 13.78645833299193413, 2.248837904296538515 ) ) ;
#9933 = VECTOR ( 'NONE', #4327, 1000.000000000000000 ) ;
#9934 = VERTEX_POINT ( 'NONE', #1337 ) ;
#9935 = STYLED_ITEM ( 'NONE', ( #7653 ), #6551 ) ;
#9936 = CARTESIAN_POINT ( 'NONE',  ( -62.86468353124999453, 12.01562499965860198, 1.500000000000002220 ) ) ;
#9937 = LINE ( 'NONE', #3990, #9364 ) ;
#9938 = EDGE_CURVE ( 'NONE', #3002, #8372, #3457, .T. ) ;
#9939 = CARTESIAN_POINT ( 'NONE',  ( 0.3609765494018736809, 0.2499999999999982792, 1.888098105530059190 ) ) ;
#9940 = ORIENTED_EDGE ( 'NONE', *, *, #8649, .F. ) ;
#9941 = CARTESIAN_POINT ( 'NONE',  ( -62.26794919243111082, 11.07366454968462932, 0.5000000000000013323 ) ) ;
#9942 = PRESENTATION_LAYER_ASSIGNMENT (  '', '', ( #8172 ) ) ;
#9943 = ORIENTED_EDGE ( 'NONE', *, *, #10676, .F. ) ;
#9944 = UNCERTAINTY_MEASURE_WITH_UNIT (LENGTH_MEASURE( 1.000000000000000082E-05 ), #9927, 'distance_accuracy_value', 'NONE');
#9945 = DIRECTION ( 'NONE',  ( 1.000000000000000000, 0.000000000000000000, 0.000000000000000000 ) ) ;
#9946 = CARTESIAN_POINT ( 'NONE',  ( -62.99999999999998579, 9.354166666666666075, 0.9226497308103756012 ) ) ;
#9947 = DIRECTION ( 'NONE',  ( -1.000000000000000000, -0.000000000000000000, -0.000000000000000000 ) ) ;
#9948 = CARTESIAN_POINT ( 'NONE',  ( -60.99999999999998579, 14.98958333265053611, 0.9226497308103762673 ) ) ;
#9949 = CYLINDRICAL_SURFACE ( 'NONE', #2630, 0.9999999999999981126 ) ;
#9950 = EDGE_CURVE ( 'NONE', #2208, #7538, #6368, .T. ) ;
#9951 = CYLINDRICAL_SURFACE ( 'NONE', #10624, 0.9999999999999981126 ) ;
#9952 = CARTESIAN_POINT ( 'NONE',  ( -61.99999999999998579, 11.32812499965860020, 2.498450539062049724 ) ) ;
#9953 = LINE ( 'NONE', #9895, #9809 ) ;
#9954 = VERTEX_POINT ( 'NONE', #10661 ) ;
#9955 = CARTESIAN_POINT ( 'NONE',  ( -61.49999999999998579, 9.260416665983870033, 0.6339745962155628467 ) ) ;
#9956 = ORIENTED_EDGE ( 'NONE', *, *, #7256, .F. ) ;
#9957 = CARTESIAN_POINT ( 'NONE',  ( -60.99999999999998579, 13.71874999931720218, 1.500000000000002220 ) ) ;
#9958 = CARTESIAN_POINT ( 'NONE',  ( -61.56765823437498852, 14.28645833299193413, 2.248837904296538515 ) ) ;
#9959 = EDGE_CURVE ( 'NONE', #1714, #5618, #7259, .T. ) ;
#9960 = DIRECTION ( 'NONE',  ( -1.000000000000000000, -0.000000000000000000, -0.000000000000000000 ) ) ;
#9961 = DIRECTION ( 'NONE',  ( -0.000000000000000000, -0.000000000000000000, 1.000000000000000000 ) ) ;
#9962 = CARTESIAN_POINT ( 'NONE',  ( -61.99999999999998579, 16.00000000000000000, 0.5000000000000041078 ) ) ;
#9963 = CARTESIAN_POINT ( 'NONE',  ( -62.86468353124999453, 12.01562499965860198, 1.500000000000002220 ) ) ;
#9964 = CARTESIAN_POINT ( 'NONE',  ( -61.99999999999998579, 15.20312499965860020, 0.5015494609379544944 ) ) ;
#9965 = CARTESIAN_POINT ( 'NONE',  ( -61.56765823437498852, 16.03645833299193768, 2.248837904296538515 ) ) ;
#9966 = CARTESIAN_POINT ( 'NONE',  ( -62.49999999999998579, 15.55208333265053611, 0.6339745962155627357 ) ) ;
#9967 = DIRECTION ( 'NONE',  ( 0.000000000000000000, 0.000000000000000000, 1.000000000000000000 ) ) ;
#9968 = EDGE_LOOP ( 'NONE', ( #7398, #1918, #880, #865 ) ) ;
#9969 = LINE ( 'NONE', #2252, #7614 ) ;
#9970 = CARTESIAN_POINT ( 'NONE',  ( -57.99999999999998579, -14.00000000000001243, 0.000000000000000000 ) ) ;
#9971 = AXIS2_PLACEMENT_3D ( 'NONE', #6589, #7361, #10746 ) ;
#9972 = CARTESIAN_POINT ( 'NONE',  ( -61.99999999999999289, 14.39062499965860198, 0.5015494609379544944 ) ) ;
#9973 = CARTESIAN_POINT ( 'NONE',  ( -62.86468353124998742, 9.223958332991935904, 1.999225269531025972 ) ) ;
#9974 = EDGE_CURVE ( 'NONE', #8454, #6686, #4653, .T. ) ;
#9975 = CARTESIAN_POINT ( 'NONE',  ( -61.13531646874997705, 15.86979166632526628, 1.999225269531026417 ) ) ;
#9976 = DIRECTION ( 'NONE',  ( 0.000000000000000000, 0.000000000000000000, 1.000000000000000000 ) ) ;
#9977 = ORIENTED_EDGE ( 'NONE', *, *, #4185, .F. ) ;
#9978 = CARTESIAN_POINT ( 'NONE',  ( -62.49999999999998579, 13.66666666666666785, 2.366025403784441483 ) ) ;
#9979 = CARTESIAN_POINT ( 'NONE',  ( -62.99999999999998579, 11.07291666598386826, 0.9226497308103756012 ) ) ;
#9980 = ADVANCED_FACE ( 'NONE', ( #1438 ), #4814, .F. ) ;
#9981 = CARTESIAN_POINT ( 'NONE',  ( -60.99999999999998579, 11.73958333265053788, 0.9226497308103762673 ) ) ;
#9982 = DIRECTION ( 'NONE',  ( 0.000000000000000000, 0.000000000000000000, -1.000000000000000000 ) ) ;
#9983 = CARTESIAN_POINT ( 'NONE',  ( -61.56765823437498852, 14.53645833299193413, 2.248837904296538515 ) ) ;
#9984 = DIRECTION ( 'NONE',  ( -0.000000000000000000, -1.000000000000000000, -0.000000000000000000 ) ) ;
#9985 = ORIENTED_EDGE ( 'NONE', *, *, #1448, .F. ) ;
#9986 = VECTOR ( 'NONE', #324, 1000.000000000000000 ) ;
#9987 = CIRCLE ( 'NONE', #8049, 20.00000000000000355 ) ;
#9988 = CARTESIAN_POINT ( 'NONE',  ( -61.13531646874998415, 11.41145833299193590, 1.000774730468978468 ) ) ;
#9989 = CARTESIAN_POINT ( 'NONE',  ( -60.99999999999998579, 12.23958333265053611, 0.9226497308103762673 ) ) ;
#9990 = CARTESIAN_POINT ( 'NONE',  ( -61.56765823437498142, 15.18229166632526805, 0.7511620957034663704 ) ) ;
#9991 = ORIENTED_EDGE ( 'NONE', *, *, #5725, .T. ) ;
#9992 = CARTESIAN_POINT ( 'NONE',  ( -62.26794919243111082, 11.17633545031536890, 2.500000000000003109 ) ) ;
#9993 = ORIENTED_EDGE ( 'NONE', *, *, #5031, .F. ) ;
#9994 = CARTESIAN_POINT ( 'NONE',  ( -61.49999999999998579, 9.427083332650536107, 2.366025403784441927 ) ) ;
#9995 = CARTESIAN_POINT ( 'NONE',  ( -62.49999999999998579, 9.833333333333332149, 0.6339745962155627357 ) ) ;
#9996 = DIRECTION ( 'NONE',  ( 0.000000000000000000, 0.000000000000000000, -1.000000000000000000 ) ) ;
#9997 = CARTESIAN_POINT ( 'NONE',  ( -61.49999999999998579, 8.208333333333333925, 2.366025403784441927 ) ) ;
#9998 = VECTOR ( 'NONE', #5340, 1000.000000000000000 ) ;
#9999 = EDGE_CURVE ( 'NONE', #7538, #930, #6608, .T. ) ;
#10000 = CARTESIAN_POINT ( 'NONE',  ( -62.49999999999998579, 9.135416665983868256, 2.366025403784441483 ) ) ;
#10001 = CARTESIAN_POINT ( 'NONE',  ( -61.13531646874998415, 11.41145833299193590, 1.000774730468978468 ) ) ;
#10002 = FACE_OUTER_BOUND ( 'NONE', #1939, .T. ) ;
#10003 = VERTEX_POINT ( 'NONE', #9882 ) ;
#10004 = LINE ( 'NONE', #3277, #8883 ) ;
#10005 = ADVANCED_FACE ( 'NONE', ( #3052 ), #6500, .T. ) ;
#10006 = CARTESIAN_POINT ( 'NONE',  ( 0.5477065543514070267, 2.408992218395923449E-16, 1.934182851860892116 ) ) ;
#10007 = CARTESIAN_POINT ( 'NONE',  ( 144.0000000000000284, -5.500000000000000000, 3.000000000000000000 ) ) ;
#10008 = CARTESIAN_POINT ( 'NONE',  ( -61.13531646874998415, 14.05729166632526805, 1.999225269531026417 ) ) ;
#10009 = DIRECTION ( 'NONE',  ( -0.000000000000000000, -0.000000000000000000, -1.000000000000000000 ) ) ;
#10010 = CARTESIAN_POINT ( 'NONE',  ( -62.86468353124998032, 13.24479166632526983, 1.000774730468978024 ) ) ;
#10011 = CARTESIAN_POINT ( 'NONE',  ( -62.43234176562498305, 15.97395833299193590, 0.7511620957034662593 ) ) ;
#10012 = PLANE ( 'NONE',  #8494 ) ;
#10013 = ITEM_DEFINED_TRANSFORMATION ( 'NONE', 'NONE', #1052,  #2307 ) ;
#10014 = CARTESIAN_POINT ( 'NONE',  ( -61.99999999999998579, -8.000000000000000000, 2.500000000000003109 ) ) ;
#10015 = CARTESIAN_POINT ( 'NONE',  ( -61.13531646874998415, 8.411458332991934128, 1.000774730468978468 ) ) ;
#10016 = FACE_OUTER_BOUND ( 'NONE', #6271, .T. ) ;
#10017 = VERTEX_POINT ( 'NONE', #2321 ) ;
#10018 = CARTESIAN_POINT ( 'NONE',  ( 140.0000000000000284, 8.000000000000000000, 6.000000000000000000 ) ) ;
#10019 = LINE ( 'NONE', #4898, #2531 ) ;
#10020 = CARTESIAN_POINT ( 'NONE',  ( -61.99999999999999289, 14.64062499965859843, 0.5015494609379544944 ) ) ;
#10021 = CARTESIAN_POINT ( 'NONE',  ( -62.43234176562499016, 9.994791666325268054, 2.248837904296538071 ) ) ;
#10022 = CARTESIAN_POINT ( 'NONE',  ( -61.99999999999999289, 8.140624999658601979, 0.5015494609379544944 ) ) ;
#10023 = CARTESIAN_POINT ( 'NONE',  ( -77.99999999999998579, 0.000000000000000000, 5.000000000000000000 ) ) ;
#10024 = ORIENTED_EDGE ( 'NONE', *, *, #2995, .T. ) ;
#10025 = CARTESIAN_POINT ( 'NONE',  ( -62.99999999999998579, 13.60416666666666607, 0.9226497308103756012 ) ) ;
#10026 = CARTESIAN_POINT ( 'NONE',  ( -61.13531646874997705, 8.161458332991934128, 1.000774730468978468 ) ) ;
#10027 = EDGE_CURVE ( 'NONE', #4585, #3431, #498, .T. ) ;
#10028 = CARTESIAN_POINT ( 'NONE',  ( -61.49999999999998579, 11.42708333265053611, 2.366025403784441927 ) ) ;
#10029 = CARTESIAN_POINT ( 'NONE',  ( 0.000000000000000000, 0.000000000000000000, 0.000000000000000000 ) ) ;
#10030 = ADVANCED_FACE ( 'NONE', ( #8945 ), #5759, .T. ) ;
#10031 = CARTESIAN_POINT ( 'NONE',  ( -61.13531646874998415, 13.32812499965860020, 1.500000000000002220 ) ) ;
#10032 =( NAMED_UNIT ( * ) SI_UNIT ( $, .STERADIAN. ) SOLID_ANGLE_UNIT ( ) );
#10033 = ORIENTED_EDGE ( 'NONE', *, *, #6394, .F. ) ;
#10034 = CARTESIAN_POINT ( 'NONE',  ( -62.43234176562498305, 10.97395833299193590, 0.7511620957034662593 ) ) ;
#10035 = PLANE ( 'NONE',  #3171 ) ;
#10036 = CARTESIAN_POINT ( 'NONE',  ( 2.924531576190634356E-30, -2.388061258337343593E-14, 2.000000000000000000 ) ) ;
#10037 = ORIENTED_EDGE ( 'NONE', *, *, #658, .F. ) ;
#10038 = DIRECTION ( 'NONE',  ( 0.000000000000000000, -1.000000000000000000, 0.000000000000000000 ) ) ;
#10039 = EDGE_CURVE ( 'NONE', #8495, #6754, #9937, .T. ) ;
#10040 = ORIENTED_EDGE ( 'NONE', *, *, #3970, .F. ) ;
#10041 = CARTESIAN_POINT ( 'NONE',  ( -61.99999999999998579, 15.56249999999999822, 0.5000000000000013323 ) ) ;
#10042 = CARTESIAN_POINT ( 'NONE',  ( -61.99999999999998579, 10.81249999999999822, 0.3452994616207497591 ) ) ;
#10043 = CARTESIAN_POINT ( 'NONE',  ( -44.00000000000000711, -14.00000000000000888, 3.000000000000000000 ) ) ;
#10044 = DIRECTION ( 'NONE',  ( -0.000000000000000000, -1.000000000000000000, -0.000000000000000000 ) ) ;
#10045 = UNCERTAINTY_MEASURE_WITH_UNIT (LENGTH_MEASURE( 1.000000000000000082E-05 ), #6328, 'distance_accuracy_value', 'NONE');
#10046 = CARTESIAN_POINT ( 'NONE',  ( -62.86468353124998742, 13.03645833299193235, 1.999225269531025972 ) ) ;
#10047 = CARTESIAN_POINT ( 'NONE',  ( -61.99999999999998579, 12.03124999931720041, 0.5000000000000013323 ) ) ;
#10048 = EDGE_LOOP ( 'NONE', ( #6524, #9051, #2225, #10151 ) ) ;
#10049 = CARTESIAN_POINT ( 'NONE',  ( -62.49999999999998579, 15.33333333333333393, 0.6339745962155627357 ) ) ;
#10050 = VERTEX_POINT ( 'NONE', #9101 ) ;
#10051 = CARTESIAN_POINT ( 'NONE',  ( 150.0000000000000000, -8.000000000000000000, 6.000000000000000000 ) ) ;
#10052 = CARTESIAN_POINT ( 'NONE',  ( -62.86468353124998742, 15.72395833299193768, 1.999225269531025972 ) ) ;
#10053 = CARTESIAN_POINT ( 'NONE',  ( -61.99999999999998579, 11.81249999999999822, 0.5000000000000013323 ) ) ;
#10054 = SURFACE_STYLE_USAGE ( .BOTH. , #6678 ) ;
#10055 = DIRECTION ( 'NONE',  ( 0.000000000000000000, 1.000000000000000000, 0.000000000000000000 ) ) ;
#10056 = CARTESIAN_POINT ( 'NONE',  ( -61.13531646874997705, 12.91145833299193590, 1.000774730468978468 ) ) ;
#10057 = CARTESIAN_POINT ( 'NONE',  ( -61.13531646874998415, 15.39062499965860020, 1.500000000000002220 ) ) ;
#10058 = CARTESIAN_POINT ( 'NONE',  ( -60.99999999999998579, 15.00000000000000000, 1.500000000000002220 ) ) ;
#10059 = CARTESIAN_POINT ( 'NONE',  ( -61.73205080756886076, 13.41741454900182973, 2.500000000000003109 ) ) ;
#10060 = CIRCLE ( 'NONE', #7585, 6.000000000000005329 ) ;
#10061 = CARTESIAN_POINT ( 'NONE',  ( -62.43234176562498305, 8.223958332991934128, 0.7511620957034662593 ) ) ;
#10062 = FACE_BOUND ( 'NONE', #5216, .T. ) ;
#10063 = ORIENTED_EDGE ( 'NONE', *, *, #1671, .T. ) ;
#10064 = CARTESIAN_POINT ( 'NONE',  ( -61.99999999999998579, 11.90624999931720041, 2.500000000000002665 ) ) ;
#10065 = LINE ( 'NONE', #5846, #5178 ) ;
#10066 = CARTESIAN_POINT ( 'NONE',  ( -61.13531646874997705, 13.84895833299193413, 1.000774730468978468 ) ) ;
#10067 = CARTESIAN_POINT ( 'NONE',  ( -62.86468353124999453, 9.203124999658600203, 1.500000000000002220 ) ) ;
#10068 = CARTESIAN_POINT ( 'NONE',  ( -77.99999999999998579, -11.50000000000000711, 8.000000000000000000 ) ) ;
#10069 = ORIENTED_EDGE ( 'NONE', *, *, #4658, .F. ) ;
#10070 = CARTESIAN_POINT ( 'NONE',  ( -61.49999999999998579, 13.79166666666666785, 0.6339745962155628467 ) ) ;
#10071 = CARTESIAN_POINT ( 'NONE',  ( -62.86468353124998032, 8.994791666325268054, 1.000774730468978024 ) ) ;
#10072 = SHAPE_REPRESENTATION_RELATIONSHIP ( 'NONE' , 'NONE' ,  #6156, #6440 ) ;
#10073 = CARTESIAN_POINT ( 'NONE',  ( -62.99999999999998579, 12.32291666598386826, 0.9226497308103756012 ) ) ;
#10074 = PLANE ( 'NONE',  #2352 ) ;
#10075 = VECTOR ( 'NONE', #9017, 1000.000000000000000 ) ;
#10076 = CIRCLE ( 'NONE', #2820, 2.000000000000000000 ) ;
#10077 = CARTESIAN_POINT ( 'NONE',  ( -62.43234176562498305, 13.41145833299193413, 0.7511620957034662593 ) ) ;
#10078 = DIRECTION ( 'NONE',  ( -0.000000000000000000, -0.000000000000000000, 1.000000000000000000 ) ) ;
#10079 = EDGE_LOOP ( 'NONE', ( #4460, #9215, #1042, #3396, #1602, #3014, #10567, #4516, #4593 ) ) ;
#10080 = AXIS2_PLACEMENT_3D ( 'NONE', #5577, #2301, #531 ) ;
#10081 = ADVANCED_FACE ( 'NONE', ( #7437 ), #9829, .T. ) ;
#10082 = CARTESIAN_POINT ( 'NONE',  ( -62.86468353124998032, 13.49479166632526805, 1.000774730468978246 ) ) ;
#10083 = CARTESIAN_POINT ( 'NONE',  ( -61.49999999999998579, 11.42708333265053611, 2.366025403784441927 ) ) ;
#10084 = AXIS2_PLACEMENT_3D ( 'NONE', #4918, #10919, #8316 ) ;
#10085 = DIRECTION ( 'NONE',  ( 0.000000000000000000, -0.000000000000000000, 1.000000000000000000 ) ) ;
#10086 = APPLICATION_CONTEXT ( 'automotive_design' ) ;
#10087 = ORIENTED_EDGE ( 'NONE', *, *, #7541, .T. ) ;
#10088 = CARTESIAN_POINT ( 'NONE',  ( -61.99999999999998579, 12.43749999999999822, 2.500000000000002665 ) ) ;
#10089 = AXIS2_PLACEMENT_3D ( 'NONE', #8821, #1207, #4586 ) ;
#10090 = ORIENTED_EDGE ( 'NONE', *, *, #7319, .F. ) ;
#10091 = CARTESIAN_POINT ( 'NONE',  ( -60.99999999999998579, 10.47916666666666607, 2.077350269189628840 ) ) ;
#10092 = ORIENTED_EDGE ( 'NONE', *, *, #2504, .F. ) ;
#10093 = CARTESIAN_POINT ( 'NONE',  ( -61.13531646874998415, 8.369791666325268054, 1.999225269531026417 ) ) ;
#10094 = DIRECTION ( 'NONE',  ( 0.000000000000000000, -1.000000000000000000, 0.000000000000000000 ) ) ;
#10095 = VECTOR ( 'NONE', #1355, 1000.000000000000000 ) ;
#10096 = EDGE_CURVE ( 'NONE', #4846, #562, #2822, .T. ) ;
#10097 = CARTESIAN_POINT ( 'NONE',  ( -61.99999999999998579, 13.45312499965860376, 0.5015494609379544944 ) ) ;
#10098 = PRESENTATION_LAYER_ASSIGNMENT (  '', '', ( #365 ) ) ;
#10099 = LINE ( 'NONE', #4967, #10861 ) ;
#10100 = VERTEX_POINT ( 'NONE', #2480 ) ;
#10101 = ORIENTED_EDGE ( 'NONE', *, *, #10904, .F. ) ;
#10102 = CARTESIAN_POINT ( 'NONE',  ( -62.43234176562499016, 14.99479166632526805, 2.248837904296538071 ) ) ;
#10103 = CARTESIAN_POINT ( 'NONE',  ( -61.99999999999998579, 8.000000000000000000, 1.500000000000002220 ) ) ;
#10104 = CARTESIAN_POINT ( 'NONE',  ( -62.99999999999998579, 8.104166666666667851, 0.9226497308103756012 ) ) ;
#10105 =( BOUNDED_CURVE ( )  B_SPLINE_CURVE ( 2, ( #5004, #3292, #638, #3137, #7520, #5741, #9916, #7414, #10064 ),
 .UNSPECIFIED., .F., .T. ) 
 B_SPLINE_CURVE_WITH_KNOTS ( ( 3, 2, 2, 2, 3 ),
 ( 0.4453125000000000000, 0.4479166666666666852, 0.4531250000000000000, 0.4583333333333333148, 0.4609375000000000000 ),
 .UNSPECIFIED. ) 
 CURVE ( )  GEOMETRIC_REPRESENTATION_ITEM ( )  RATIONAL_B_SPLINE_CURVE ( ( 0.9330127018922194093, 0.9330127018922194093, 1.000000000000000000, 0.8660254037844387076, 1.000000000000000000, 0.8660254037844387076, 1.000000000000000000, 0.9330127018922194093, 0.9330127018922194093 ) ) 
 REPRESENTATION_ITEM ( '' )  );
#10106 = CARTESIAN_POINT ( 'NONE',  ( -77.99999999999998579, 0.000000000000000000, 13.00000000000000178 ) ) ;
#10107 = CARTESIAN_POINT ( 'NONE',  ( -61.56765823437498852, 13.09895833299193413, 2.248837904296538515 ) ) ;
#10108 = CARTESIAN_POINT ( 'NONE',  ( -61.56765823437498852, 15.84895833299193590, 2.248837904296538515 ) ) ;
#10109 = DIRECTION ( 'NONE',  ( 0.000000000000000000, 0.000000000000000000, -1.000000000000000000 ) ) ;
#10110 = CARTESIAN_POINT ( 'NONE',  ( -61.99999999999998579, 8.562500000000000000, 0.5000000000000013323 ) ) ;
#10111 = CARTESIAN_POINT ( 'NONE',  ( -61.99999999999998579, 9.203124999658601979, 0.5015494609379544944 ) ) ;
#10112 = CARTESIAN_POINT ( 'NONE',  ( -61.99999999999998579, 16.00000000000000000, 1.500000000000002220 ) ) ;
#10113 = ORIENTED_EDGE ( 'NONE', *, *, #3403, .F. ) ;
#10114 = LINE ( 'NONE', #1846, #9382 ) ;
#10115 = DIRECTION ( 'NONE',  ( 0.9961946980917455452, 1.067350013832299055E-17, 0.08715574274765831853 ) ) ;
#10116 = CARTESIAN_POINT ( 'NONE',  ( -61.13531646874997705, 16.05729166632526628, 1.999225269531026417 ) ) ;
#10117 = CARTESIAN_POINT ( 'NONE',  ( -61.13531646874998415, 11.80729166632526805, 1.999225269531026417 ) ) ;
#10118 = CARTESIAN_POINT ( 'NONE',  ( -62.43234176562498305, 15.97395833299193590, 0.7511620957034662593 ) ) ;
#10119 = CARTESIAN_POINT ( 'NONE',  ( 0.5000000000000000000, 0.000000000000000000, 0.000000000000000000 ) ) ;
#10120 = ORIENTED_EDGE ( 'NONE', *, *, #9319, .F. ) ;
#10121 = CARTESIAN_POINT ( 'NONE',  ( -61.49999999999998579, 14.45833333333333393, 2.366025403784441927 ) ) ;
#10122 = CARTESIAN_POINT ( 'NONE',  ( -61.13531646874997705, 8.661458332991934128, 1.000774730468978468 ) ) ;
#10123 = CARTESIAN_POINT ( 'NONE',  ( -61.49999999999998579, 12.67708333265053611, 2.366025403784441927 ) ) ;
#10124 = ORIENTED_EDGE ( 'NONE', *, *, #7226, .F. ) ;
#10125 = ADVANCED_FACE ( 'NONE', ( #1701 ), #810, .T. ) ;
#10126 =( LENGTH_UNIT ( ) NAMED_UNIT ( * ) SI_UNIT ( .MILLI., .METRE. ) );
#10127 = AXIS2_PLACEMENT_3D ( 'NONE', #4131, #9923, #10908 ) ;
#10128 = CARTESIAN_POINT ( 'NONE',  ( -62.86468353124998032, 13.43229166632526628, 1.000774730468978246 ) ) ;
#10129 = ADVANCED_FACE ( 'NONE', ( #10188 ), #9207, .T. ) ;
#10130 = CARTESIAN_POINT ( 'NONE',  ( -77.99999999999998579, 11.49999999999999645, 5.000000000000000000 ) ) ;
#10131 = ORIENTED_EDGE ( 'NONE', *, *, #4320, .F. ) ;
#10132 = CARTESIAN_POINT ( 'NONE',  ( -49.99999999999998579, -10.00000000000000888, 3.000000000000000000 ) ) ;
#10133 = CARTESIAN_POINT ( 'NONE',  ( -62.86468353124999453, 13.01562499965860198, 1.500000000000002220 ) ) ;
#10134 = CARTESIAN_POINT ( 'NONE',  ( -61.99999999999998579, 16.00000000000000000, 1.500000000000002220 ) ) ;
#10135 = ORIENTED_EDGE ( 'NONE', *, *, #10589, .T. ) ;
#10136 = LINE ( 'NONE', #10036, #4957 ) ;
#10137 = ORIENTED_EDGE ( 'NONE', *, *, #10310, .F. ) ;
#10138 = CARTESIAN_POINT ( 'NONE',  ( -62.49999999999998579, 12.33333333333333393, 0.6339745962155627357 ) ) ;
#10139 = AXIS2_PLACEMENT_3D ( 'NONE', #5503, #2906, #10508 ) ;
#10140 = VECTOR ( 'NONE', #2439, 1000.000000000000000 ) ;
#10141 = ORIENTED_EDGE ( 'NONE', *, *, #6545, .F. ) ;
#10142 = CARTESIAN_POINT ( 'NONE',  ( -62.49999999999998579, 11.41666666666666785, 2.366025403784441483 ) ) ;
#10143 = ORIENTED_EDGE ( 'NONE', *, *, #9423, .T. ) ;
#10144 = CARTESIAN_POINT ( 'NONE',  ( -62.86468353124999453, 8.515624999658601979, 1.500000000000002220 ) ) ;
#10145 = DIRECTION ( 'NONE',  ( 0.000000000000000000, -1.000000000000000000, 0.000000000000000000 ) ) ;
#10146 = VECTOR ( 'NONE', #8410, 1000.000000000000000 ) ;
#10147 = EDGE_CURVE ( 'NONE', #10397, #5874, #3180, .T. ) ;
#10148 = VECTOR ( 'NONE', #1018, 999.9999999999998863 ) ;
#10149 = CARTESIAN_POINT ( 'NONE',  ( -62.43234176562499016, 13.80729166632526805, 2.248837904296538071 ) ) ;
#10150 = CARTESIAN_POINT ( 'NONE',  ( -62.99999999999998579, 12.82291666598386826, 0.9226497308103756012 ) ) ;
#10151 = ORIENTED_EDGE ( 'NONE', *, *, #7699, .T. ) ;
#10152 = CARTESIAN_POINT ( 'NONE',  ( -144.9999999999999432, 8.000000000000000000, 3.000000000000000000 ) ) ;
#10153 = ADVANCED_FACE ( 'NONE', ( #8427 ), #3259, .T. ) ;
#10154 = ORIENTED_EDGE ( 'NONE', *, *, #8180, .F. ) ;
#10155 = CIRCLE ( 'NONE', #3427, 1.099999999999989875 ) ;
#10156 = CARTESIAN_POINT ( 'NONE',  ( -60.99999999999998579, 13.21874999931720396, 1.500000000000002220 ) ) ;
#10157 = CARTESIAN_POINT ( 'NONE',  ( -61.99999999999998579, 15.26562499965860020, 2.498450539062049724 ) ) ;
#10158 = DIRECTION ( 'NONE',  ( 0.000000000000000000, 0.000000000000000000, 1.000000000000000000 ) ) ;
#10159 = CARTESIAN_POINT ( 'NONE',  ( 0.000000000000000000, 2.500000000000000000, 3.000000000000000000 ) ) ;
#10160 = CARTESIAN_POINT ( 'NONE',  ( -62.43234176562499016, 12.30729166632526805, 2.248837904296538071 ) ) ;
#10161 = CARTESIAN_POINT ( 'NONE',  ( -61.99999999999998579, 8.390624999658601979, 0.5015494609379544944 ) ) ;
#10162 = LINE ( 'NONE', #2560, #6900 ) ;
#10163 = DIRECTION ( 'NONE',  ( 0.000000000000000000, 0.000000000000000000, -1.000000000000000000 ) ) ;
#10164 = CARTESIAN_POINT ( 'NONE',  ( -61.56765823437498852, 9.098958332991935904, 2.248837904296538515 ) ) ;
#10165 = CARTESIAN_POINT ( 'NONE',  ( -61.49999999999998579, 15.67708333265053611, 2.366025403784441927 ) ) ;
#10166 = ORIENTED_EDGE ( 'NONE', *, *, #6152, .F. ) ;
#10167 = AXIS2_PLACEMENT_3D ( 'NONE', #6227, #8499, #1777 ) ;
#10168 = CARTESIAN_POINT ( 'NONE',  ( -120.0000000000000000, -15.00000000000001421, 5.000000000000004441 ) ) ;
#10169 = DIRECTION ( 'NONE',  ( -0.000000000000000000, -0.000000000000000000, 1.000000000000000000 ) ) ;
#10170 =( BOUNDED_CURVE ( )  B_SPLINE_CURVE ( 2, ( #7778, #8552, #160, #6889, #10260, #3544, #2669, #6944, #10320 ),
 .UNSPECIFIED., .F., .T. ) 
 B_SPLINE_CURVE_WITH_KNOTS ( ( 3, 2, 2, 2, 3 ),
 ( 0.3515625000000000000, 0.3541666666666666852, 0.3593750000000000000, 0.3645833333333333148, 0.3671875000000000000 ),
 .UNSPECIFIED. ) 
 CURVE ( )  GEOMETRIC_REPRESENTATION_ITEM ( )  RATIONAL_B_SPLINE_CURVE ( ( 0.9330127018922194093, 0.9330127018922194093, 1.000000000000000000, 0.8660254037844387076, 1.000000000000000000, 0.8660254037844387076, 1.000000000000000000, 0.9330127018922194093, 0.9330127018922194093 ) ) 
 REPRESENTATION_ITEM ( '' )  );
#10171 = CARTESIAN_POINT ( 'NONE',  ( -61.99999999999999289, 15.39062499965860020, 0.5015494609379544944 ) ) ;
#10172 = EDGE_CURVE ( 'NONE', #5931, #5580, #2646, .T. ) ;
#10173 = CARTESIAN_POINT ( 'NONE',  ( -62.86468353124999453, 11.70312499965860198, 1.500000000000002220 ) ) ;
#10174 = CARTESIAN_POINT ( 'NONE',  ( -62.43234176562499016, 16.05729166632526628, 2.248837904296538071 ) ) ;
#10175 = CARTESIAN_POINT ( 'NONE',  ( -62.99999999999998579, 13.09374999931720396, 1.500000000000001998 ) ) ;
#10176 = ORIENTED_EDGE ( 'NONE', *, *, #821, .T. ) ;
#10177 = CARTESIAN_POINT ( 'NONE',  ( -62.49999999999998579, 15.58333333333333393, 0.6339745962155627357 ) ) ;
#10178 = CARTESIAN_POINT ( 'NONE',  ( -61.99999999999999289, 8.703124999658601979, 0.5015494609379544944 ) ) ;
#10179 = CARTESIAN_POINT ( 'NONE',  ( -62.99999999999998579, 12.84374999931720396, 1.500000000000001998 ) ) ;
#10180 = CARTESIAN_POINT ( 'NONE',  ( -62.99999999999998579, 14.62500000000000000, 1.500000000000001998 ) ) ;
#10181 = FACE_OUTER_BOUND ( 'NONE', #1370, .T. ) ;
#10182 = CARTESIAN_POINT ( 'NONE',  ( -61.13531646874998415, 11.82812499965860198, 1.500000000000002220 ) ) ;
#10183 = DIRECTION ( 'NONE',  ( -0.000000000000000000, -0.000000000000000000, 1.000000000000000000 ) ) ;
#10184 = EDGE_CURVE ( 'NONE', #5900, #4466, #1756, .T. ) ;
#10185 = EDGE_LOOP ( 'NONE', ( #4300, #5827, #8869, #3257 ) ) ;
#10186 = CARTESIAN_POINT ( 'NONE',  ( -77.99999999999998579, -11.50000000000000711, -2.000000000000001332 ) ) ;
#10187 = CARTESIAN_POINT ( 'NONE',  ( -61.13531646874998415, 12.39062499965860198, 1.500000000000002220 ) ) ;
#10188 = FACE_OUTER_BOUND ( 'NONE', #6456, .T. ) ;
#10189 = CARTESIAN_POINT ( 'NONE',  ( -61.99999999999998579, 9.531249999317203958, 0.3452994616207497591 ) ) ;
#10190 = ORIENTED_EDGE ( 'NONE', *, *, #9781, .F. ) ;
#10191 = ADVANCED_FACE ( 'NONE', ( #4973 ), #2585, .T. ) ;
#10192 = CARTESIAN_POINT ( 'NONE',  ( -49.99999999999998579, 3.999999999999980904, -2.000000000000000000 ) ) ;
#10193 = ORIENTED_EDGE ( 'NONE', *, *, #1647, .F. ) ;
#10194 = DIRECTION ( 'NONE',  ( 0.000000000000000000, 0.000000000000000000, -1.000000000000000000 ) ) ;
#10195 = CARTESIAN_POINT ( 'NONE',  ( -62.86468353124998742, 10.97395833299193768, 1.999225269531025972 ) ) ;
#10196 = SHAPE_REPRESENTATION_RELATIONSHIP ( 'NONE' , 'NONE' ,  #5800, #4690 ) ;
#10197 = VERTEX_POINT ( 'NONE', #4188 ) ;
#10198 = CARTESIAN_POINT ( 'NONE',  ( -62.86468353124998742, 9.036458332991934128, 1.999225269531025972 ) ) ;
#10199 = CARTESIAN_POINT ( 'NONE',  ( -61.99999999999998579, 14.18750000000000000, 2.500000000000002665 ) ) ;
#10200 = CARTESIAN_POINT ( 'NONE',  ( -61.99999999999998579, 13.57812499965860020, 2.498450539062049724 ) ) ;
#10201 = EDGE_LOOP ( 'NONE', ( #2625, #5979, #7182, #5533 ) ) ;
#10202 = CARTESIAN_POINT ( 'NONE',  ( -62.49999999999998579, 9.333333333333333925, 0.6339745962155627357 ) ) ;
#10203 = ORIENTED_EDGE ( 'NONE', *, *, #6711, .F. ) ;
#10204 = CARTESIAN_POINT ( 'NONE',  ( -62.26794919243111082, 11.64508544963257286, 2.500000000000006217 ) ) ;
#10205 = CARTESIAN_POINT ( 'NONE',  ( -62.86468353124999453, 15.45312499965860020, 1.500000000000002220 ) ) ;
#10206 = CARTESIAN_POINT ( 'NONE',  ( -61.99999999999998579, 16.00000000000000000, 1.500000000000002220 ) ) ;
#10207 = LINE ( 'NONE', #5995, #1923 ) ;
#10208 = CARTESIAN_POINT ( 'NONE',  ( -62.99999999999998579, 8.875000000000001776, 1.500000000000001998 ) ) ;
#10209 = CARTESIAN_POINT ( 'NONE',  ( -61.99999999999999289, 12.45312499965860020, 0.5015494609379544944 ) ) ;
#10210 = CARTESIAN_POINT ( 'NONE',  ( -61.56765823437498852, 8.536458332991934128, 2.248837904296538515 ) ) ;
#10211 = EDGE_CURVE ( 'NONE', #4762, #4311, #4664, .T. ) ;
#10212 = CARTESIAN_POINT ( 'NONE',  ( -49.99999999999998579, -8.000000000000000000, 83.15773105863907233 ) ) ;
#10213 = CARTESIAN_POINT ( 'NONE',  ( -60.99999999999998579, 13.44791666598387003, 2.077350269189628840 ) ) ;
#10214 = CARTESIAN_POINT ( 'NONE',  ( -61.99999999999998579, 9.328124999658600203, 2.498450539062049724 ) ) ;
#10215 = CARTESIAN_POINT ( 'NONE',  ( -61.99999999999998579, 16.00000000000000000, 1.500000000000002220 ) ) ;
#10216 = ORIENTED_EDGE ( 'NONE', *, *, #6766, .T. ) ;
#10217 = FACE_OUTER_BOUND ( 'NONE', #10344, .T. ) ;
#10218 = CARTESIAN_POINT ( 'NONE',  ( -62.26794919243111082, 11.42633545031537068, 2.500000000000006217 ) ) ;
#10219 = CARTESIAN_POINT ( 'NONE',  ( -62.43234176562498305, 15.41145833299193590, 0.7511620957034662593 ) ) ;
#10220 = CARTESIAN_POINT ( 'NONE',  ( -61.99999999999998579, 10.89062499965860020, 0.5015494609379544944 ) ) ;
#10221 = CARTESIAN_POINT ( 'NONE',  ( -62.86468353124999453, 9.473958332991934128, 1.999225269531025750 ) ) ;
#10222 = CARTESIAN_POINT ( 'NONE',  ( -62.26794919243111082, 13.14508544963257286, 2.500000000000003109 ) ) ;
#10223 = ORIENTED_EDGE ( 'NONE', *, *, #6128, .T. ) ;
#10224 = CARTESIAN_POINT ( 'NONE',  ( -62.99999999999998579, 15.35416666666666785, 0.9226497308103756012 ) ) ;
#10225 = DIRECTION ( 'NONE',  ( -1.000000000000000000, -0.000000000000000000, -0.000000000000000000 ) ) ;
#10226 = CARTESIAN_POINT ( 'NONE',  ( -60.99999999999998579, 12.69791666598386826, 2.077350269189628840 ) ) ;
#10227 = LINE ( 'NONE', #5118, #9998 ) ;
#10228 = EDGE_LOOP ( 'NONE', ( #8042, #10934 ) ) ;
#10229 = ADVANCED_FACE ( 'NONE', ( #7590 ), #10035, .F. ) ;
#10230 = CARTESIAN_POINT ( 'NONE',  ( -78.99999999999998579, 11.49999999999999645, 5.000000000000000000 ) ) ;
#10231 =( BOUNDED_CURVE ( )  B_SPLINE_CURVE ( 2, ( #229, #7680, #114, #62, #5215, #3614, #6174, #4378, #7791 ),
 .UNSPECIFIED., .F., .T. ) 
 B_SPLINE_CURVE_WITH_KNOTS ( ( 3, 2, 2, 2, 3 ),
 ( 0.7265625000000000000, 0.7291666666666666297, 0.7343750000000000000, 0.7395833333333333703, 0.7421875000000000000 ),
 .UNSPECIFIED. ) 
 CURVE ( )  GEOMETRIC_REPRESENTATION_ITEM ( )  RATIONAL_B_SPLINE_CURVE ( ( 0.9330127018922194093, 0.9330127018922194093, 1.000000000000000000, 0.8660254037844387076, 1.000000000000000000, 0.8660254037844387076, 1.000000000000000000, 0.9330127018922194093, 0.9330127018922194093 ) ) 
 REPRESENTATION_ITEM ( '' )  );
#10232 = VECTOR ( 'NONE', #10078, 1000.000000000000000 ) ;
#10233 = CARTESIAN_POINT ( 'NONE',  ( -62.86468353124999453, 11.20312499965860020, 1.500000000000002220 ) ) ;
#10234 = FILL_AREA_STYLE_COLOUR ( '', #7062 ) ;
#10235 = LINE ( 'NONE', #4979, #10709 ) ;
#10236 = EDGE_LOOP ( 'NONE', ( #2399, #6418, #6237, #6606 ) ) ;
#10237 = CARTESIAN_POINT ( 'NONE',  ( 150.0000000000000284, -8.000000000000000000, 3.000000000000000000 ) ) ;
#10238 = CARTESIAN_POINT ( 'NONE',  ( -62.86468353124998742, 12.78645833299193413, 1.999225269531025972 ) ) ;
#10239 = CARTESIAN_POINT ( 'NONE',  ( -61.73205080756886076, 11.52008544963257108, 0.5000000000000014433 ) ) ;
#10240 = CIRCLE ( 'NONE', #5987, 6.000000000000005329 ) ;
#10241 = CARTESIAN_POINT ( 'NONE',  ( -62.49999999999998579, 8.885416665983868256, 2.366025403784441483 ) ) ;
#10242 = VERTEX_POINT ( 'NONE', #3362 ) ;
#10243 = LINE ( 'NONE', #3310, #1589 ) ;
#10244 = AXIS2_PLACEMENT_3D ( 'NONE', #8435, #10145, #979 ) ;
#10245 = ORIENTED_EDGE ( 'NONE', *, *, #8322, .T. ) ;
#10246 = CARTESIAN_POINT ( 'NONE',  ( -62.99999999999998579, 12.37500000000000000, 1.500000000000001998 ) ) ;
#10247 = CARTESIAN_POINT ( 'NONE',  ( -62.86468353124999453, 11.45312499965860020, 1.500000000000002220 ) ) ;
#10248 = FILL_AREA_STYLE_COLOUR ( '', #2649 ) ;
#10249 = VECTOR ( 'NONE', #5942, 1000.000000000000000 ) ;
#10250 = EDGE_LOOP ( 'NONE', ( #923, #2434, #7443, #347 ) ) ;
#10251 = CARTESIAN_POINT ( 'NONE',  ( -61.99999999999998579, 8.578124999658601979, 2.498450539062049724 ) ) ;
#10252 = CARTESIAN_POINT ( 'NONE',  ( -61.99999999999997868, 10.53124999931720573, 0.5000000000000013323 ) ) ;
#10253 = VECTOR ( 'NONE', #10561, 1000.000000000000000 ) ;
#10254 = CARTESIAN_POINT ( 'NONE',  ( -61.13531646874998415, 13.36979166632526628, 1.999225269531026417 ) ) ;
#10255 = CARTESIAN_POINT ( 'NONE',  ( -49.99999999999998579, -18.00000000000001066, 3.000000000000000000 ) ) ;
#10256 = EDGE_LOOP ( 'NONE', ( #2195, #3712, #2326, #4431 ) ) ;
#10257 = FACE_OUTER_BOUND ( 'NONE', #5479, .T. ) ;
#10258 = AXIS2_PLACEMENT_3D ( 'NONE', #1952, #4549, #3727 ) ;
#10259 = VERTEX_POINT ( 'NONE', #6866 ) ;
#10260 = CARTESIAN_POINT ( 'NONE',  ( -62.99999999999998579, 10.87500000000000000, 1.500000000000001998 ) ) ;
#10261 = EDGE_CURVE ( 'NONE', #6858, #6924, #2418, .T. ) ;
#10262 = CARTESIAN_POINT ( 'NONE',  ( -61.56765823437498142, 14.61979166632526805, 0.7511620957034663704 ) ) ;
#10263 = AXIS2_PLACEMENT_3D ( 'NONE', #3586, #10305, #6932 ) ;
#10264 = CARTESIAN_POINT ( 'NONE',  ( -105.0000000000000000, 2.500000000000000000, 4.000000000000000000 ) ) ;
#10265 = LINE ( 'NONE', #8557, #1389 ) ;
#10266 = CARTESIAN_POINT ( 'NONE',  ( -61.99999999999999289, 13.95312499965860198, 0.5015494609379544944 ) ) ;
#10267 = CARTESIAN_POINT ( 'NONE',  ( -61.99999999999998579, 9.265624999658600203, 2.498450539062049724 ) ) ;
#10268 = DIRECTION ( 'NONE',  ( 0.000000000000000000, 0.000000000000000000, -1.000000000000000000 ) ) ;
#10269 = CARTESIAN_POINT ( 'NONE',  ( -61.99999999999998579, 16.00000000000000000, 0.5000000000000041078 ) ) ;
#10270 = CARTESIAN_POINT ( 'NONE',  ( -62.86468353124998032, 9.494791666325269830, 1.000774730468978246 ) ) ;
#10271 = DIRECTION ( 'NONE',  ( 0.000000000000000000, 1.000000000000000000, 0.000000000000000000 ) ) ;
#10272 = ORIENTED_EDGE ( 'NONE', *, *, #10968, .F. ) ;
#10273 = CARTESIAN_POINT ( 'NONE',  ( -61.99999999999998579, 16.00000000000000000, 2.500000000000000444 ) ) ;
#10274 = CARTESIAN_POINT ( 'NONE',  ( -61.99999999999998579, 16.00000000000000000, 1.500000000000002220 ) ) ;
#10275 = CIRCLE ( 'NONE', #4237, 1.000000000000000888 ) ;
#10276 = EDGE_CURVE ( 'NONE', #8261, #5305, #4090, .T. ) ;
#10277 = PRODUCT_DEFINITION_FORMATION_WITH_SPECIFIED_SOURCE ( 'ANY', '', #3510, .NOT_KNOWN. ) ;
#10278 = CARTESIAN_POINT ( 'NONE',  ( -61.99999999999999289, 15.89062499965860198, 0.5015494609379544944 ) ) ;
#10279 = CARTESIAN_POINT ( 'NONE',  ( -62.86468353124999453, 11.20312499965860020, 1.500000000000002220 ) ) ;
#10280 = CARTESIAN_POINT ( 'NONE',  ( -61.13531646874997705, 8.598958332991934128, 1.000774730468978468 ) ) ;
#10281 = VERTEX_POINT ( 'NONE', #32 ) ;
#10282 = CARTESIAN_POINT ( 'NONE',  ( -60.99999999999998579, 15.27083333333333393, 0.9226497308103762673 ) ) ;
#10283 = CARTESIAN_POINT ( 'NONE',  ( -62.43234176562499016, 10.05729166632526805, 2.248837904296538071 ) ) ;
#10284 = CARTESIAN_POINT ( 'NONE',  ( 0.000000000000000000, 0.000000000000000000, 0.000000000000000000 ) ) ;
#10285 = CARTESIAN_POINT ( 'NONE',  ( -61.99999999999998579, 13.78124999931720218, 0.3452994616207497591 ) ) ;
#10286 = DIRECTION ( 'NONE',  ( 1.000000000000000000, 0.000000000000000000, 0.000000000000000000 ) ) ;
#10287 = VERTEX_POINT ( 'NONE', #5971 ) ;
#10288 = EDGE_CURVE ( 'NONE', #3072, #8746, #5130, .T. ) ;
#10289 = CARTESIAN_POINT ( 'NONE',  ( -62.26794919243111082, 11.57366454968462932, 0.5000000000000013323 ) ) ;
#10290 = EDGE_CURVE ( 'NONE', #6091, #767, #7540, .T. ) ;
#10291 = CARTESIAN_POINT ( 'NONE',  ( -61.56765823437498142, 11.86979166632526805, 0.7511620957034663704 ) ) ;
#10292 = CARTESIAN_POINT ( 'NONE',  ( 145.0000000000000284, 5.500000000000000000, 3.000000000000000000 ) ) ;
#10293 = APPLICATION_CONTEXT ( 'automotive_design' ) ;
#10294 = CARTESIAN_POINT ( 'NONE',  ( -60.99999999999998579, 12.97916666666666607, 2.077350269189628840 ) ) ;
#10295 = VERTEX_POINT ( 'NONE', #7931 ) ;
#10296 = EDGE_CURVE ( 'NONE', #1159, #5429, #7374, .T. ) ;
#10297 = CARTESIAN_POINT ( 'NONE',  ( -61.28647452029539267, 16.00000000000000000, 0.7993707187018740390 ) ) ;
#10298 = CARTESIAN_POINT ( 'NONE',  ( -62.86468353124998032, 12.99479166632526805, 1.000774730468978246 ) ) ;
#10299 = SURFACE_STYLE_FILL_AREA ( #137 ) ;
#10300 = CARTESIAN_POINT ( 'NONE',  ( -60.99999999999998579, 11.00000000000000000, 1.500000000000002220 ) ) ;
#10301 = CARTESIAN_POINT ( 'NONE',  ( -60.99999999999998579, 9.739583332650536107, 0.9226497308103762673 ) ) ;
#10302 = PRODUCT_DEFINITION ( 'UNKNOWN', '', #5499, #5604 ) ;
#10303 = VERTEX_POINT ( 'NONE', #9416 ) ;
#10304 =( BOUNDED_CURVE ( )  B_SPLINE_CURVE ( 2, ( #4858, #5530, #647, #8985, #8932, #486, #8207, #1325, #598 ),
 .UNSPECIFIED., .F., .T. ) 
 B_SPLINE_CURVE_WITH_KNOTS ( ( 3, 2, 2, 2, 3 ),
 ( 0.6328125000000000000, 0.6354166666666666297, 0.6406250000000000000, 0.6458333333333333703, 0.6484375000000000000 ),
 .UNSPECIFIED. ) 
 CURVE ( )  GEOMETRIC_REPRESENTATION_ITEM ( )  RATIONAL_B_SPLINE_CURVE ( ( 0.9330127018922194093, 0.9330127018922194093, 1.000000000000000000, 0.8660254037844387076, 1.000000000000000000, 0.8660254037844387076, 1.000000000000000000, 0.9330127018922194093, 0.9330127018922194093 ) ) 
 REPRESENTATION_ITEM ( '' )  );
#10305 = DIRECTION ( 'NONE',  ( -2.478176394252581696E-17, 1.000000000000000000, 0.000000000000000000 ) ) ;
#10306 = CARTESIAN_POINT ( 'NONE',  ( -60.99999999999998579, 9.947916665983870033, 2.077350269189628840 ) ) ;
#10307 = CARTESIAN_POINT ( 'NONE',  ( -61.56765823437498142, 11.61979166632526805, 0.7511620957034663704 ) ) ;
#10308 = SURFACE_SIDE_STYLE ('',( #9424 ) ) ;
#10309 = ORIENTED_EDGE ( 'NONE', *, *, #1317, .T. ) ;
#10310 = EDGE_CURVE ( 'NONE', #8229, #10601, #6144, .T. ) ;
#10311 = CARTESIAN_POINT ( 'NONE',  ( -61.13531646874998415, 8.869791666325268054, 1.999225269531026417 ) ) ;
#10312 = FACE_OUTER_BOUND ( 'NONE', #2748, .T. ) ;
#10313 = CARTESIAN_POINT ( 'NONE',  ( -61.56765823437498852, 14.59895833299193413, 2.248837904296538515 ) ) ;
#10314 = CARTESIAN_POINT ( 'NONE',  ( -62.26794919243111082, 12.79241454900183150, 0.5000000000000013323 ) ) ;
#10315 = ORIENTED_EDGE ( 'NONE', *, *, #2401, .F. ) ;
#10316 = VECTOR ( 'NONE', #1353, 1000.000000000000000 ) ;
#10317 = DIRECTION ( 'NONE',  ( 1.000000000000000000, 0.000000000000000000, 0.000000000000000000 ) ) ;
#10318 = VECTOR ( 'NONE', #6262, 1000.000000000000000 ) ;
#10319 = ORIENTED_EDGE ( 'NONE', *, *, #7387, .T. ) ;
#10320 = CARTESIAN_POINT ( 'NONE',  ( -61.99999999999998579, 10.93750000000000000, 2.500000000000002665 ) ) ;
#10321 = CARTESIAN_POINT ( 'NONE',  ( -61.49999999999998579, 8.291666666666666075, 0.6339745962155628467 ) ) ;
#10322 = CARTESIAN_POINT ( 'NONE',  ( -62.26794919243112503, 8.792414549001835056, 0.5000000000000022204 ) ) ;
#10323 = CARTESIAN_POINT ( 'NONE',  ( -60.99999999999998579, 12.44791666598386826, 2.077350269189628840 ) ) ;
#10324 = EDGE_CURVE ( 'NONE', #353, #9106, #1146, .T. ) ;
#10325 = FACE_OUTER_BOUND ( 'NONE', #757, .T. ) ;
#10326 = AXIS2_PLACEMENT_3D ( 'NONE', #363, #3919, #3976 ) ;
#10327 = CARTESIAN_POINT ( 'NONE',  ( -62.43234176562499016, 14.30729166632526983, 2.248837904296538071 ) ) ;
#10328 = VECTOR ( 'NONE', #2813, 1000.000000000000000 ) ;
#10329 = CARTESIAN_POINT ( 'NONE',  ( -61.13531646874998415, 8.578124999658601979, 1.500000000000002220 ) ) ;
#10330 = DIRECTION ( 'NONE',  ( 0.000000000000000000, 0.000000000000000000, -1.000000000000000000 ) ) ;
#10331 = CARTESIAN_POINT ( 'NONE',  ( 7.300000000000000711, 0.000000000000000000, 1.000000000000000000 ) ) ;
#10332 = CARTESIAN_POINT ( 'NONE',  ( -62.86468353124998742, 11.03645833299193413, 1.999225269531025972 ) ) ;
#10333 = CARTESIAN_POINT ( 'NONE',  ( 0.000000000000000000, 0.2499999999999982792, -1.312875263449799323 ) ) ;
#10334 = VERTEX_POINT ( 'NONE', #5240 ) ;
#10335 = DIRECTION ( 'NONE',  ( 1.000000000000000000, 0.000000000000000000, 0.000000000000000000 ) ) ;
#10336 = EDGE_CURVE ( 'NONE', #2581, #2979, #8933, .T. ) ;
#10337 = DIRECTION ( 'NONE',  ( 1.000000000000000000, 0.000000000000000000, 0.000000000000000000 ) ) ;
#10338 =( BOUNDED_CURVE ( )  B_SPLINE_CURVE ( 2, ( #8731, #3611, #7956, #10560, #1171, #2957, #2066, #6342, #10386 ),
 .UNSPECIFIED., .F., .F. ) 
 B_SPLINE_CURVE_WITH_KNOTS ( ( 3, 2, 2, 2, 3 ),
 ( 0.4609375000000000000, 0.4635416666666666852, 0.4687500000000000000, 0.4739583333333333148, 0.4765625000000000000 ),
 .UNSPECIFIED. ) 
 CURVE ( )  GEOMETRIC_REPRESENTATION_ITEM ( )  RATIONAL_B_SPLINE_CURVE ( ( 0.9330127018922194093, 0.9330127018922194093, 1.000000000000000000, 0.8660254037844387076, 1.000000000000000000, 0.8660254037844387076, 1.000000000000000000, 0.9330127018922194093, 0.9330127018922194093 ) ) 
 REPRESENTATION_ITEM ( '' )  );
#10339 = VECTOR ( 'NONE', #5519, 1000.000000000000000 ) ;
#10340 = LINE ( 'NONE', #9506, #1103 ) ;
#10341 = CARTESIAN_POINT ( 'NONE',  ( -62.43234176562499016, 12.74479166632526805, 2.248837904296538071 ) ) ;
#10342 = CARTESIAN_POINT ( 'NONE',  ( -62.86468353124999453, 8.223958332991934128, 1.999225269531025750 ) ) ;
#10343 = CARTESIAN_POINT ( 'NONE',  ( -61.73205080756886076, 9.667414549001833279, 2.500000000000000000 ) ) ;
#10344 = EDGE_LOOP ( 'NONE', ( #93, #4987, #983, #5473 ) ) ;
#10345 = CARTESIAN_POINT ( 'NONE',  ( -60.99999999999998579, 15.22916666666666607, 2.077350269189628840 ) ) ;
#10346 = CARTESIAN_POINT ( 'NONE',  ( -61.13531646874997705, 9.661458332991934128, 1.000774730468978468 ) ) ;
#10347 = CARTESIAN_POINT ( 'NONE',  ( -61.13531646874998415, 15.09895833299193413, 1.000774730468978468 ) ) ;
#10348 = AXIS2_PLACEMENT_3D ( 'NONE', #4942, #9173, #2441 ) ;
#10349 = CARTESIAN_POINT ( 'NONE',  ( -60.99999999999998579, 13.23958333265053611, 0.9226497308103762673 ) ) ;
#10350 = DIRECTION ( 'NONE',  ( -1.000000000000000000, -0.000000000000000000, -0.000000000000000000 ) ) ;
#10351 = ORIENTED_EDGE ( 'NONE', *, *, #1485, .F. ) ;
#10352 = DIRECTION ( 'NONE',  ( 0.000000000000000000, -0.000000000000000000, 1.000000000000000000 ) ) ;
#10353 = CARTESIAN_POINT ( 'NONE',  ( -61.56765823437498142, 11.11979166632526805, 0.7511620957034663704 ) ) ;
#10354 = FACE_OUTER_BOUND ( 'NONE', #9707, .T. ) ;
#10355 = CARTESIAN_POINT ( 'NONE',  ( -61.73205080756886076, 13.05133545031537068, 0.5000000000000014433 ) ) ;
#10356 = ORIENTED_EDGE ( 'NONE', *, *, #3057, .F. ) ;
#10357 = CARTESIAN_POINT ( 'NONE',  ( -60.99999999999998579, 11.27083333333333393, 0.9226497308103762673 ) ) ;
#10358 = EDGE_CURVE ( 'NONE', #2581, #6912, #8818, .T. ) ;
#10359 = LINE ( 'NONE', #6141, #2526 ) ;
#10360 = CARTESIAN_POINT ( 'NONE',  ( -61.13531646874998415, 14.39062499965860020, 1.500000000000002220 ) ) ;
#10361 = CARTESIAN_POINT ( 'NONE',  ( -60.99999999999998579, 10.97916666666666607, 2.077350269189628840 ) ) ;
#10362 = CARTESIAN_POINT ( 'NONE',  ( -60.99999999999998579, 9.489583332650537884, 0.9226497308103762673 ) ) ;
#10363 = ADVANCED_FACE ( 'NONE', ( #1024 ), #10414, .T. ) ;
#10364 = ORIENTED_EDGE ( 'NONE', *, *, #1928, .T. ) ;
#10365 = CARTESIAN_POINT ( 'NONE',  ( -60.99999999999998579, 13.50000000000000000, 1.500000000000002220 ) ) ;
#10366 = CARTESIAN_POINT ( 'NONE',  ( -62.99999999999998579, 13.35416666666666785, 0.9226497308103756012 ) ) ;
#10367 = CARTESIAN_POINT ( 'NONE',  ( -61.13531646874998415, 10.84895833299193590, 1.000774730468978468 ) ) ;
#10368 = FILL_AREA_STYLE ('',( #10248 ) ) ;
#10369 = ORIENTED_EDGE ( 'NONE', *, *, #5877, .F. ) ;
#10370 = CARTESIAN_POINT ( 'NONE',  ( -61.13531646874998415, 10.41145833299193413, 1.000774730468978468 ) ) ;
#10371 = DIRECTION ( 'NONE',  ( 0.000000000000000000, 0.000000000000000000, 1.000000000000000000 ) ) ;
#10372 = CARTESIAN_POINT ( 'NONE',  ( -61.13531646874998415, 15.11979166632526628, 1.999225269531026417 ) ) ;
#10373 = CARTESIAN_POINT ( 'NONE',  ( -61.99999999999998579, 16.00000000000000000, 2.500000000000000444 ) ) ;
#10374 = ORIENTED_EDGE ( 'NONE', *, *, #602, .T. ) ;
#10375 = CARTESIAN_POINT ( 'NONE',  ( -62.99999999999998579, 9.354166666666666075, 0.9226497308103756012 ) ) ;
#10376 = ADVANCED_FACE ( 'NONE', ( #1082 ), #310, .T. ) ;
#10377 = APPLICATION_CONTEXT ( 'automotive_design' ) ;
#10378 = EDGE_LOOP ( 'NONE', ( #7335, #2650, #9476, #9007 ) ) ;
#10379 = CARTESIAN_POINT ( 'NONE',  ( -61.49999999999998579, 12.67708333265053611, 2.366025403784441927 ) ) ;
#10380 = CARTESIAN_POINT ( 'NONE',  ( -60.99999999999998579, 8.270833333333332149, 0.9226497308103762673 ) ) ;
#10381 = CARTESIAN_POINT ( 'NONE',  ( -37.99999999999999289, -14.00000000000000888, 5.000000000000000000 ) ) ;
#10382 = CARTESIAN_POINT ( 'NONE',  ( -61.99999999999998579, 9.156249999317203958, 2.500000000000002665 ) ) ;
#10383 = CARTESIAN_POINT ( 'NONE',  ( -61.49999999999998579, 10.67708333265053611, 2.366025403784441927 ) ) ;
#10384 = CARTESIAN_POINT ( 'NONE',  ( -61.13531646874997705, 13.91145833299193413, 1.000774730468978468 ) ) ;
#10385 = CARTESIAN_POINT ( 'NONE',  ( -61.13531646874998415, 8.328124999658601979, 1.500000000000002220 ) ) ;
#10386 = CARTESIAN_POINT ( 'NONE',  ( -61.99999999999998579, 12.03124999931720041, 0.5000000000000013323 ) ) ;
#10387 = CARTESIAN_POINT ( 'NONE',  ( -77.99999999999998579, -11.50000000000000711, 8.000000000000000000 ) ) ;
#10388 = CARTESIAN_POINT ( 'NONE',  ( -62.43234176562499016, 10.05729166632526805, 2.248837904296538071 ) ) ;
#10389 = CARTESIAN_POINT ( 'NONE',  ( -61.99999999999998579, 15.65624999931720218, 2.500000000000002665 ) ) ;
#10390 = EDGE_LOOP ( 'NONE', ( #8438, #2114, #8930, #8802 ) ) ;
#10391 = CARTESIAN_POINT ( 'NONE',  ( 1.299999999999999156, 2.449293598294706414E-16, 2.000000000000000000 ) ) ;
#10392 = DIRECTION ( 'NONE',  ( -0.000000000000000000, -1.000000000000000000, -0.000000000000000000 ) ) ;
#10393 = CARTESIAN_POINT ( 'NONE',  ( -61.73205080756886076, 15.69866454968462932, 2.500000000000003109 ) ) ;
#10394 = CARTESIAN_POINT ( 'NONE',  ( -61.13531646874998415, 12.30729166632526628, 1.999225269531026417 ) ) ;
#10395 = CARTESIAN_POINT ( 'NONE',  ( -61.13531646874997705, 9.348958332991937681, 1.000774730468978468 ) ) ;
#10396 = DIRECTION ( 'NONE',  ( -0.000000000000000000, 1.000000000000000000, -0.000000000000000000 ) ) ;
#10397 = VERTEX_POINT ( 'NONE', #3581 ) ;
#10398 = CARTESIAN_POINT ( 'NONE',  ( -61.99999999999998579, 16.00000000000000000, 1.500000000000002220 ) ) ;
#10399 = CARTESIAN_POINT ( 'NONE',  ( -61.56765823437498852, 9.598958332991934128, 2.248837904296538515 ) ) ;
#10400 = DIRECTION ( 'NONE',  ( 1.000000000000000000, 0.000000000000000000, 0.000000000000000000 ) ) ;
#10401 = CARTESIAN_POINT ( 'NONE',  ( -61.99999999999998579, 15.89062499965860198, 0.5015494609379544944 ) ) ;
#10402 = CARTESIAN_POINT ( 'NONE',  ( -60.99999999999998579, 14.23958333265053611, 0.9226497308103762673 ) ) ;
#10403 = CARTESIAN_POINT ( 'NONE',  ( -61.99999999999998579, 14.56249999999999822, 0.5000000000000013323 ) ) ;
#10404 = EDGE_LOOP ( 'NONE', ( #8286, #4756, #1197, #5674 ) ) ;
#10405 = SHAPE_REPRESENTATION ( 'clamp', ( #2307 ), #6012 ) ;
#10406 = CARTESIAN_POINT ( 'NONE',  ( -62.99999999999998579, 11.60416666666666785, 0.9226497308103756012 ) ) ;
#10407 = CARTESIAN_POINT ( 'NONE',  ( -62.86468353124999453, 10.95312499965860020, 1.500000000000002220 ) ) ;
#10408 = CARTESIAN_POINT ( 'NONE',  ( -61.13531646874998415, 8.828124999658601979, 1.500000000000002220 ) ) ;
#10409 = LINE ( 'NONE', #2426, #9272 ) ;
#10410 = ORIENTED_EDGE ( 'NONE', *, *, #6658, .F. ) ;
#10411 = CARTESIAN_POINT ( 'NONE',  ( -62.99999999999998579, 11.37500000000000000, 1.500000000000001998 ) ) ;
#10412 = LINE ( 'NONE', #1979, #6265 ) ;
#10413 = CARTESIAN_POINT ( 'NONE',  ( -62.86468353124998742, 14.28645833299193413, 1.999225269531025972 ) ) ;
#10414 = PLANE ( 'NONE',  #9561 ) ;
#10415 = CARTESIAN_POINT ( 'NONE',  ( -60.99999999999998579, 9.989583332650534331, 0.9226497308103762673 ) ) ;
#10416 = ORIENTED_EDGE ( 'NONE', *, *, #7522, .F. ) ;
#10417 = CARTESIAN_POINT ( 'NONE',  ( -60.99999999999998579, 13.97916666666666785, 2.077350269189628840 ) ) ;
#10418 = EDGE_CURVE ( 'NONE', #10259, #6385, #4290, .T. ) ;
#10419 = FACE_OUTER_BOUND ( 'NONE', #6815, .T. ) ;
#10420 = CARTESIAN_POINT ( 'NONE',  ( -61.56765823437498852, 11.03645833299193590, 2.248837904296538515 ) ) ;
#10421 = CARTESIAN_POINT ( 'NONE',  ( -60.99999999999998579, 16.00000000000000000, 1.500000000000002220 ) ) ;
#10422 = ADVANCED_FACE ( 'NONE', ( #9589 ), #6928, .T. ) ;
#10423 = ORIENTED_EDGE ( 'NONE', *, *, #3265, .F. ) ;
#10424 = AXIS2_PLACEMENT_3D ( 'NONE', #5408, #429, #4521 ) ;
#10425 = CARTESIAN_POINT ( 'NONE',  ( -61.13531646874998415, 10.64062499965860198, 1.500000000000002220 ) ) ;
#10426 = LINE ( 'NONE', #2829, #1214 ) ;
#10427 = CARTESIAN_POINT ( 'NONE',  ( -62.86468353124998742, 14.03645833299193590, 1.999225269531025972 ) ) ;
#10428 = DIRECTION ( 'NONE',  ( -1.000000000000000000, 8.673617379884033500E-16, 0.000000000000000000 ) ) ;
#10429 = ORIENTED_EDGE ( 'NONE', *, *, #9084, .F. ) ;
#10430 = LINE ( 'NONE', #6223, #6575 ) ;
#10431 = AXIS2_PLACEMENT_3D ( 'NONE', #4983, #4929, #8384 ) ;
#10432 = AXIS2_PLACEMENT_3D ( 'NONE', #322, #5424, #9714 ) ;
#10433 = VERTEX_POINT ( 'NONE', #4347 ) ;
#10434 = CARTESIAN_POINT ( 'NONE',  ( -149.9999999999999716, -8.000000000000000000, 3.000000000000000000 ) ) ;
#10435 = CARTESIAN_POINT ( 'NONE',  ( -61.49999999999998579, 9.041666666666666075, 0.6339745962155628467 ) ) ;
#10436 = DIRECTION ( 'NONE',  ( -1.000000000000000000, -0.000000000000000000, -0.000000000000000000 ) ) ;
#10437 = CARTESIAN_POINT ( 'NONE',  ( -57.99999999999998579, 0.000000000000000000, -0.1418111474832477736 ) ) ;
#10438 = CARTESIAN_POINT ( 'NONE',  ( -62.49999999999998579, 8.916666666666666075, 2.366025403784441483 ) ) ;
#10439 = CARTESIAN_POINT ( 'NONE',  ( -61.56765823437498142, 14.43229166632526983, 0.7511620957034663704 ) ) ;
#10440 = EDGE_CURVE ( 'NONE', #8694, #4585, #6983, .T. ) ;
#10441 = CIRCLE ( 'NONE', #4396, 1.099999999999989875 ) ;
#10442 = CARTESIAN_POINT ( 'NONE',  ( -61.13531646874998415, 9.557291666325269830, 1.999225269531026417 ) ) ;
#10443 = CARTESIAN_POINT ( 'NONE',  ( -144.9999999999999432, 8.000000000000000000, 3.000000000000000000 ) ) ;
#10444 = DIRECTION ( 'NONE',  ( -0.000000000000000000, 0.000000000000000000, 1.000000000000000000 ) ) ;
#10445 = CARTESIAN_POINT ( 'NONE',  ( -61.13531646874998415, 9.890624999658601979, 1.500000000000002220 ) ) ;
#10446 = AXIS2_PLACEMENT_3D ( 'NONE', #9819, #2394, #5784 ) ;
#10447 = CARTESIAN_POINT ( 'NONE',  ( -61.99999999999998579, 13.56249999999999822, 0.5000000000000013323 ) ) ;
#10448 = ORIENTED_EDGE ( 'NONE', *, *, #3988, .T. ) ;
#10449 = CARTESIAN_POINT ( 'NONE',  ( -61.99999999999998579, 14.06250000000000000, 0.5000000000000013323 ) ) ;
#10450 = CARTESIAN_POINT ( 'NONE',  ( -60.99999999999998579, 15.25000000000000000, 1.500000000000002220 ) ) ;
#10451 = VECTOR ( 'NONE', #762, 1000.000000000000000 ) ;
#10452 = CARTESIAN_POINT ( 'NONE',  ( -61.73205080756886076, 15.80133545031536713, 0.5000000000000014433 ) ) ;
#10453 = CARTESIAN_POINT ( 'NONE',  ( -61.13531646874998415, 12.80729166632526805, 1.999225269531026417 ) ) ;
#10454 = CARTESIAN_POINT ( 'NONE',  ( -61.99999999999999289, 8.390624999658601979, 0.5015494609379544944 ) ) ;
#10455 = DIRECTION ( 'NONE',  ( 0.000000000000000000, 1.000000000000000000, 0.000000000000000000 ) ) ;
#10456 = ORIENTED_EDGE ( 'NONE', *, *, #5195, .F. ) ;
#10457 = CARTESIAN_POINT ( 'NONE',  ( -60.99999999999998579, 15.77083333333333215, 0.9226497308103762673 ) ) ;
#10458 = CARTESIAN_POINT ( 'NONE',  ( -61.56765823437498142, 9.432291666325268054, 0.7511620957034663704 ) ) ;
#10459 = APPLICATION_PROTOCOL_DEFINITION ( 'draft international standard', 'automotive_design', 1998, #4191 ) ;
#10460 = CARTESIAN_POINT ( 'NONE',  ( -61.13531646874998415, 15.59895833299193590, 1.000774730468978468 ) ) ;
#10461 = VECTOR ( 'NONE', #4657, 1000.000000000000000 ) ;
#10462 = CARTESIAN_POINT ( 'NONE',  ( -62.99999999999998579, 14.61458333265053611, 2.077350269189627952 ) ) ;
#10463 = CARTESIAN_POINT ( 'NONE',  ( -114.9999999999999147, -43.00000000000000000, -2.000000000000000000 ) ) ;
#10464 = ORIENTED_EDGE ( 'NONE', *, *, #2830, .T. ) ;
#10465 = FILL_AREA_STYLE ('',( #3572 ) ) ;
#10466 = ORIENTED_EDGE ( 'NONE', *, *, #6463, .F. ) ;
#10467 = CARTESIAN_POINT ( 'NONE',  ( -62.86468353124999453, 12.47395833299193413, 1.999225269531025750 ) ) ;
#10468 = CARTESIAN_POINT ( 'NONE',  ( -62.86468353124998032, 8.932291666325268054, 1.000774730468978246 ) ) ;
#10469 = AXIS2_PLACEMENT_3D ( 'NONE', #8950, #4711, #504 ) ;
#10470 = LINE ( 'NONE', #10585, #4815 ) ;
#10471 = ORIENTED_EDGE ( 'NONE', *, *, #4038, .T. ) ;
#10472 = CARTESIAN_POINT ( 'NONE',  ( -62.49999999999998579, 12.08333333333333393, 0.6339745962155627357 ) ) ;
#10473 = CARTESIAN_POINT ( 'NONE',  ( -61.99999999999998579, 15.93749999999999645, 2.500000000000002665 ) ) ;
#10474 = CARTESIAN_POINT ( 'NONE',  ( -61.56765823437498852, 14.59895833299193413, 2.248837904296538515 ) ) ;
#10475 =( BOUNDED_CURVE ( )  B_SPLINE_CURVE ( 2, ( #7039, #9419, #3699, #10417, #9654, #1926, #1086, #143, #9477 ),
 .UNSPECIFIED., .F., .T. ) 
 B_SPLINE_CURVE_WITH_KNOTS ( ( 3, 2, 2, 2, 3 ),
 ( 0.7421875000000000000, 0.7447916666666666297, 0.7500000000000000000, 0.7552083333333333703, 0.7578125000000000000 ),
 .UNSPECIFIED. ) 
 CURVE ( )  GEOMETRIC_REPRESENTATION_ITEM ( )  RATIONAL_B_SPLINE_CURVE ( ( 0.9330127018922194093, 0.9330127018922194093, 1.000000000000000000, 0.8660254037844387076, 1.000000000000000000, 0.8660254037844387076, 1.000000000000000000, 0.9330127018922194093, 0.9330127018922194093 ) ) 
 REPRESENTATION_ITEM ( '' )  );
#10476 = EDGE_CURVE ( 'NONE', #2070, #10833, #1611, .T. ) ;
#10477 = FILL_AREA_STYLE ('',( #4749 ) ) ;
#10478 = CARTESIAN_POINT ( 'NONE',  ( -60.99999999999998579, 11.02083333333333393, 0.9226497308103762673 ) ) ;
#10479 = CARTESIAN_POINT ( 'NONE',  ( -61.49999999999998579, 10.76041666598386826, 0.6339745962155628467 ) ) ;
#10480 = ORIENTED_EDGE ( 'NONE', *, *, #5529, .F. ) ;
#10481 = CARTESIAN_POINT ( 'NONE',  ( -60.99999999999998579, 13.47916666666666785, 2.077350269189628840 ) ) ;
#10482 = CARTESIAN_POINT ( 'NONE',  ( -62.99999999999998579, 15.32291666598387003, 0.9226497308103756012 ) ) ;
#10483 = ADVANCED_FACE ( 'NONE', ( #3043 ), #10012, .T. ) ;
#10484 = CARTESIAN_POINT ( 'NONE',  ( -62.86468353124998032, 12.93229166632526805, 1.000774730468978246 ) ) ;
#10485 = DIRECTION ( 'NONE',  ( 0.000000000000000000, -0.000000000000000000, 1.000000000000000000 ) ) ;
#10486 = VERTEX_POINT ( 'NONE', #7465 ) ;
#10487 = CARTESIAN_POINT ( 'NONE',  ( -62.86468353124998032, 10.74479166632526628, 1.000774730468978246 ) ) ;
#10488 = CARTESIAN_POINT ( 'NONE',  ( -61.99999999999998579, 15.40624999931720218, 2.500000000000002665 ) ) ;
#10489 = CARTESIAN_POINT ( 'NONE',  ( -61.13531646874998415, 14.41145833299193413, 1.000774730468978468 ) ) ;
#10490 = LINE ( 'NONE', #2053, #6446 ) ;
#10491 = EDGE_LOOP ( 'NONE', ( #8710, #2697, #7991, #6694 ) ) ;
#10492 = DIRECTION ( 'NONE',  ( -0.000000000000000000, -1.000000000000000000, -0.000000000000000000 ) ) ;
#10493 = AXIS2_PLACEMENT_3D ( 'NONE', #10572, #2914, #3674 ) ;
#10494 = VERTEX_POINT ( 'NONE', #3228 ) ;
#10495 = FACE_OUTER_BOUND ( 'NONE', #10390, .T. ) ;
#10496 = CARTESIAN_POINT ( 'NONE',  ( -62.86468353124998032, 15.93229166632526805, 1.000774730468978246 ) ) ;
#10497 = CARTESIAN_POINT ( 'NONE',  ( -62.49999999999998579, 9.552083332650536107, 0.6339745962155627357 ) ) ;
#10498 = DIRECTION ( 'NONE',  ( -1.000000000000000000, -0.000000000000000000, -0.000000000000000000 ) ) ;
#10499 = CARTESIAN_POINT ( 'NONE',  ( 146.0999999999999943, 5.500000000000000000, 3.000000000000000888 ) ) ;
#10500 = EDGE_CURVE ( 'NONE', #4198, #544, #6321, .T. ) ;
#10501 = CARTESIAN_POINT ( 'NONE',  ( -62.86468353124999453, 14.76562499965860020, 1.500000000000002220 ) ) ;
#10502 = CARTESIAN_POINT ( 'NONE',  ( -61.99999999999998579, 10.39062499965860020, 0.5015494609379544944 ) ) ;
#10503 = DIRECTION ( 'NONE',  ( -0.000000000000000000, -0.000000000000000000, 1.000000000000000000 ) ) ;
#10504 = CARTESIAN_POINT ( 'NONE',  ( 0.000000000000000000, 0.2499999999999998335, 1.312875263449799101 ) ) ;
#10505 = CLOSED_SHELL ( 'NONE', ( #6905, #490, #1457, #5037, #9151, #1262, #4519, #10483 ) ) ;
#10506 = CARTESIAN_POINT ( 'NONE',  ( -61.99999999999998579, 10.32812499965860020, 2.498450539062049724 ) ) ;
#10507 = ADVANCED_FACE ( 'NONE', ( #6373 ), #8879, .T. ) ;
#10508 = DIRECTION ( 'NONE',  ( -1.000000000000000000, 0.000000000000000000, -0.000000000000000000 ) ) ;
#10509 = VERTEX_POINT ( 'NONE', #8402 ) ;
#10510 = CARTESIAN_POINT ( 'NONE',  ( -62.99999999999998579, 14.37499999999999822, 1.500000000000001998 ) ) ;
#10511 = CYLINDRICAL_SURFACE ( 'NONE', #3420, 0.9999999999999981126 ) ;
#10512 = ORIENTED_EDGE ( 'NONE', *, *, #7717, .F. ) ;
#10513 = VECTOR ( 'NONE', #2366, 1000.000000000000000 ) ;
#10514 = DIRECTION ( 'NONE',  ( -0.000000000000000000, -0.000000000000000000, -1.000000000000000000 ) ) ;
#10515 = CARTESIAN_POINT ( 'NONE',  ( -61.99999999999998579, 11.89062499965860198, 0.5015494609379544944 ) ) ;
#10516 = AXIS2_PLACEMENT_3D ( 'NONE', #616, #4768, #8276 ) ;
#10517 = CARTESIAN_POINT ( 'NONE',  ( -62.43234176562498305, 9.661458332991934128, 0.7511620957034662593 ) ) ;
#10518 = ORIENTED_EDGE ( 'NONE', *, *, #1177, .F. ) ;
#10519 = CARTESIAN_POINT ( 'NONE',  ( -61.99999999999998579, 8.531249999317203958, 0.5000000000000013323 ) ) ;
#10520 = CARTESIAN_POINT ( 'NONE',  ( -61.13531646874997705, 10.61979166632526628, 1.999225269531026417 ) ) ;
#10521 = CARTESIAN_POINT ( 'NONE',  ( -62.86468353124998742, 15.72395833299193768, 1.999225269531025972 ) ) ;
#10522 = CARTESIAN_POINT ( 'NONE',  ( -61.99999999999998579, 15.15624999931720218, 2.654700538379254571 ) ) ;
#10523 = CARTESIAN_POINT ( 'NONE',  ( -62.99999999999998579, 16.07291666598386826, 0.9226497308103756012 ) ) ;
#10524 = VERTEX_POINT ( 'NONE', #10897 ) ;
#10525 = VECTOR ( 'NONE', #7866, 1000.000000000000000 ) ;
#10526 = ORIENTED_EDGE ( 'NONE', *, *, #3812, .F. ) ;
#10527 = ADVANCED_FACE ( 'NONE', ( #6682 ), #6436, .T. ) ;
#10528 = CARTESIAN_POINT ( 'NONE',  ( -61.99999999999999289, 13.01562499965860198, 2.498450539062049724 ) ) ;
#10529 = CARTESIAN_POINT ( 'NONE',  ( -61.13531646874998415, 9.057291666325266277, 1.999225269531026417 ) ) ;
#10530 = CARTESIAN_POINT ( 'NONE',  ( -61.99999999999998579, 16.00000000000000000, 2.500000000000000444 ) ) ;
#10531 = ORIENTED_EDGE ( 'NONE', *, *, #7897, .F. ) ;
#10532 = CARTESIAN_POINT ( 'NONE',  ( -62.99999999999998579, 11.87500000000000000, 1.500000000000001998 ) ) ;
#10533 = VECTOR ( 'NONE', #9516, 1000.000000000000000 ) ;
#10534 = CARTESIAN_POINT ( 'NONE',  ( -105.0000000000000000, -2.500000000000000000, 2.000000000000000000 ) ) ;
#10535 = CARTESIAN_POINT ( 'NONE',  ( -61.56765823437498852, 14.09895833299193413, 2.248837904296538515 ) ) ;
#10536 = CARTESIAN_POINT ( 'NONE',  ( -120.0000000000000000, -15.00000000000001421, -2.000000000000000000 ) ) ;
#10537 = CARTESIAN_POINT ( 'NONE',  ( -62.49999999999998579, 10.38541666598387003, 2.366025403784441483 ) ) ;
#10538 = VERTEX_POINT ( 'NONE', #1328 ) ;
#10539 = CARTESIAN_POINT ( 'NONE',  ( -61.99999999999998579, 16.00000000000000000, 0.5000000000000041078 ) ) ;
#10540 = DIRECTION ( 'NONE',  ( 0.000000000000000000, 0.000000000000000000, 1.000000000000000000 ) ) ;
#10541 = EDGE_CURVE ( 'NONE', #3475, #6280, #1414, .T. ) ;
#10542 = CARTESIAN_POINT ( 'NONE',  ( -61.99999999999998579, 12.51562499965860198, 2.498450539062049724 ) ) ;
#10543 = FILL_AREA_STYLE ('',( #2824 ) ) ;
#10544 =( BOUNDED_CURVE ( )  B_SPLINE_CURVE ( 2, ( #3128, #3550, #106, #4161, #2727, #2608, #5152, #6837, #6893 ),
 .UNSPECIFIED., .F., .F. ) 
 B_SPLINE_CURVE_WITH_KNOTS ( ( 3, 2, 2, 2, 3 ),
 ( 0.5078125000000000000, 0.5104166666666666297, 0.5156250000000000000, 0.5208333333333333703, 0.5234375000000000000 ),
 .UNSPECIFIED. ) 
 CURVE ( )  GEOMETRIC_REPRESENTATION_ITEM ( )  RATIONAL_B_SPLINE_CURVE ( ( 0.9330127018922194093, 0.9330127018922194093, 1.000000000000000000, 0.8660254037844387076, 1.000000000000000000, 0.8660254037844387076, 1.000000000000000000, 0.9330127018922194093, 0.9330127018922194093 ) ) 
 REPRESENTATION_ITEM ( '' )  );
#10545 = ORIENTED_EDGE ( 'NONE', *, *, #7874, .T. ) ;
#10546 = CARTESIAN_POINT ( 'NONE',  ( -61.56765823437498852, 9.598958332991934128, 2.248837904296538515 ) ) ;
#10547 = LINE ( 'NONE', #2051, #7602 ) ;
#10548 = EDGE_CURVE ( 'NONE', #7156, #6540, #9178, .T. ) ;
#10549 = CARTESIAN_POINT ( 'NONE',  ( -61.13531646874998415, 14.64062499965860020, 1.500000000000002220 ) ) ;
#10550 = CARTESIAN_POINT ( 'NONE',  ( -120.0000000000000000, -15.00000000000001421, -2.000000000000000000 ) ) ;
#10551 = ORIENTED_EDGE ( 'NONE', *, *, #4352, .F. ) ;
#10552 = CARTESIAN_POINT ( 'NONE',  ( -105.0000000000000000, 2.500000000000000000, 4.000000000000000000 ) ) ;
#10553 = ORIENTED_EDGE ( 'NONE', *, *, #851, .F. ) ;
#10554 = DIRECTION ( 'NONE',  ( 0.000000000000000000, 1.000000000000000000, -5.282956808509869699E-16 ) ) ;
#10555 = CARTESIAN_POINT ( 'NONE',  ( -61.13531646874998415, 16.05729166632526983, 1.999225269531026417 ) ) ;
#10556 = DIRECTION ( 'NONE',  ( -0.000000000000000000, -0.000000000000000000, -1.000000000000000000 ) ) ;
#10557 = DIRECTION ( 'NONE',  ( 0.000000000000000000, 0.000000000000000000, 1.000000000000000000 ) ) ;
#10558 = CARTESIAN_POINT ( 'NONE',  ( -60.99999999999998579, 10.69791666598386826, 2.077350269189628840 ) ) ;
#10559 = CARTESIAN_POINT ( 'NONE',  ( -61.56765823437498142, 10.36979166632526983, 0.7511620957034663704 ) ) ;
#10560 = CARTESIAN_POINT ( 'NONE',  ( -60.99999999999998579, 11.94791666598387359, 2.077350269189628840 ) ) ;
#10561 = DIRECTION ( 'NONE',  ( -0.000000000000000000, 1.000000000000000000, -0.000000000000000000 ) ) ;
#10562 = CARTESIAN_POINT ( 'NONE',  ( -62.86468353124998742, 10.03645833299193235, 1.999225269531025972 ) ) ;
#10563 = DIRECTION ( 'NONE',  ( 0.000000000000000000, 1.000000000000000000, 0.000000000000000000 ) ) ;
#10564 = ORIENTED_EDGE ( 'NONE', *, *, #5591, .T. ) ;
#10565 = CARTESIAN_POINT ( 'NONE',  ( -105.0000000000000000, -2.500000000000000000, 2.000000000000000000 ) ) ;
#10566 = CARTESIAN_POINT ( 'NONE',  ( -49.99999999999998579, -15.00000000000001243, 83.15773105863907233 ) ) ;
#10567 = ORIENTED_EDGE ( 'NONE', *, *, #8744, .T. ) ;
#10568 = DIRECTION ( 'NONE',  ( 0.000000000000000000, 0.000000000000000000, 1.000000000000000000 ) ) ;
#10569 = CARTESIAN_POINT ( 'NONE',  ( -61.13531646874998415, 12.07812499965860198, 1.500000000000002220 ) ) ;
#10570 = EDGE_CURVE ( 'NONE', #5859, #9531, #4698, .T. ) ;
#10571 = CARTESIAN_POINT ( 'NONE',  ( -61.99999999999999289, 10.76562499965860020, 2.498450539062049724 ) ) ;
#10572 = CARTESIAN_POINT ( 'NONE',  ( -61.99999999999998579, 8.000000000000000000, 1.500000000000002220 ) ) ;
#10573 = ORIENTED_EDGE ( 'NONE', *, *, #4274, .F. ) ;
#10574 = DIRECTION ( 'NONE',  ( 0.000000000000000000, 0.000000000000000000, -1.000000000000000000 ) ) ;
#10575 = CARTESIAN_POINT ( 'NONE',  ( -62.86468353124999453, 10.76562499965860020, 1.500000000000002220 ) ) ;
#10576 = CARTESIAN_POINT ( 'NONE',  ( 0.000000000000000000, 0.000000000000000000, 0.000000000000000000 ) ) ;
#10577 = CARTESIAN_POINT ( 'NONE',  ( -61.56765823437498142, 15.11979166632526805, 0.7511620957034663704 ) ) ;
#10578 = CARTESIAN_POINT ( 'NONE',  ( -60.99999999999998579, 14.19791666598387003, 2.077350269189628840 ) ) ;
#10579 = CYLINDRICAL_SURFACE ( 'NONE', #5558, 1.000000000000000000 ) ;
#10580 = ORIENTED_EDGE ( 'NONE', *, *, #10652, .F. ) ;
#10581 = DIRECTION ( 'NONE',  ( -0.000000000000000000, -1.000000000000000000, -0.000000000000000000 ) ) ;
#10582 = ORIENTED_EDGE ( 'NONE', *, *, #7753, .T. ) ;
#10583 = CARTESIAN_POINT ( 'NONE',  ( -62.86468353124998032, 12.43229166632526805, 1.000774730468978024 ) ) ;
#10584 = CARTESIAN_POINT ( 'NONE',  ( -61.13531646874998415, 8.098958332991934128, 1.000774730468978468 ) ) ;
#10585 = CARTESIAN_POINT ( 'NONE',  ( -49.99999999999998579, -10.00000000000000888, 83.15773105863907233 ) ) ;
#10586 = ORIENTED_EDGE ( 'NONE', *, *, #5376, .T. ) ;
#10587 = CARTESIAN_POINT ( 'NONE',  ( -62.49999999999998579, 12.91666666666666607, 2.366025403784441483 ) ) ;
#10588 = DIRECTION ( 'NONE',  ( -1.000000000000000000, -1.224646799147355672E-16, 0.000000000000000000 ) ) ;
#10589 = EDGE_CURVE ( 'NONE', #8768, #8566, #9705, .T. ) ;
#10590 = CARTESIAN_POINT ( 'NONE',  ( -60.99999999999998579, 9.968749999317202182, 1.500000000000002220 ) ) ;
#10591 = ORIENTED_EDGE ( 'NONE', *, *, #7722, .T. ) ;
#10592 = CYLINDRICAL_SURFACE ( 'NONE', #2798, 0.9999999999999981126 ) ;
#10593 = CARTESIAN_POINT ( 'NONE',  ( -61.99999999999998579, 13.14062499965860198, 0.5015494609379544944 ) ) ;
#10594 = DIRECTION ( 'NONE',  ( 1.000000000000000000, 0.000000000000000000, 0.000000000000000000 ) ) ;
#10595 = ORIENTED_EDGE ( 'NONE', *, *, #3784, .F. ) ;
#10596 = CARTESIAN_POINT ( 'NONE',  ( -62.86468353124998742, 10.28645833299193590, 1.999225269531025972 ) ) ;
#10597 = CARTESIAN_POINT ( 'NONE',  ( -61.73205080756886076, 12.27008544963257286, 0.5000000000000014433 ) ) ;
#10598 = AXIS2_PLACEMENT_3D ( 'NONE', #1088, #10540, #2939 ) ;
#10599 = CARTESIAN_POINT ( 'NONE',  ( -61.56765823437498142, 15.43229166632526805, 0.7511620957034663704 ) ) ;
#10600 = DIRECTION ( 'NONE',  ( 0.000000000000000000, -1.000000000000000000, -5.421010862427519705E-17 ) ) ;
#10601 = VERTEX_POINT ( 'NONE', #734 ) ;
#10602 = LINE ( 'NONE', #3654, #1060 ) ;
#10603 =( BOUNDED_CURVE ( )  B_SPLINE_CURVE ( 2, ( #6939, #10314, #2600, #10150, #876, #5935, #6721, #9275, #4255 ),
 .UNSPECIFIED., .F., .T. ) 
 B_SPLINE_CURVE_WITH_KNOTS ( ( 3, 2, 2, 2, 3 ),
 ( 0.5703125000000000000, 0.5729166666666666297, 0.5781250000000000000, 0.5833333333333333703, 0.5859375000000000000 ),
 .UNSPECIFIED. ) 
 CURVE ( )  GEOMETRIC_REPRESENTATION_ITEM ( )  RATIONAL_B_SPLINE_CURVE ( ( 0.9330127018922194093, 0.9330127018922194093, 1.000000000000000000, 0.8660254037844387076, 1.000000000000000000, 0.8660254037844387076, 1.000000000000000000, 0.9330127018922194093, 0.9330127018922194093 ) ) 
 REPRESENTATION_ITEM ( '' )  );
#10604 = VECTOR ( 'NONE', #9468, 1000.000000000000000 ) ;
#10605 = ORIENTED_EDGE ( 'NONE', *, *, #6301, .F. ) ;
#10606 = CARTESIAN_POINT ( 'NONE',  ( -61.73205080756886787, 8.801335450315370679, 0.4999999999999967804 ) ) ;
#10607 = CARTESIAN_POINT ( 'NONE',  ( -61.99999999999998579, 10.31250000000000178, 0.3452994616207497591 ) ) ;
#10608 = CARTESIAN_POINT ( 'NONE',  ( -62.99999999999998579, 9.614583332650536107, 2.077350269189627952 ) ) ;
#10609 = DIRECTION ( 'NONE',  ( -1.000000000000000000, 0.000000000000000000, -0.000000000000000000 ) ) ;
#10610 = CARTESIAN_POINT ( 'NONE',  ( 0.5000000000000000000, 0.2499999999999982792, 2.000000000000001776 ) ) ;
#10611 = CARTESIAN_POINT ( 'NONE',  ( -61.56765823437498142, 9.619791666325268054, 0.7511620957034663704 ) ) ;
#10612 = FACE_OUTER_BOUND ( 'NONE', #2949, .T. ) ;
#10613 = VECTOR ( 'NONE', #4663, 1000.000000000000000 ) ;
#10614 = CARTESIAN_POINT ( 'NONE',  ( -62.43234176562498305, 11.22395833299193590, 0.7511620957034662593 ) ) ;
#10615 = CARTESIAN_POINT ( 'NONE',  ( -44.00000000000000000, -14.00000000000000888, 5.000000000000000000 ) ) ;
#10616 = ORIENTED_EDGE ( 'NONE', *, *, #3433, .T. ) ;
#10617 = DIRECTION ( 'NONE',  ( 0.000000000000000000, 1.000000000000000000, 0.000000000000000000 ) ) ;
#10618 = DIRECTION ( 'NONE',  ( 0.000000000000000000, 0.000000000000000000, 1.000000000000000000 ) ) ;
#10619 = CIRCLE ( 'NONE', #7973, 50.00000000000000000 ) ;
#10620 = EDGE_CURVE ( 'NONE', #4626, #2204, #8351, .T. ) ;
#10621 = ORIENTED_EDGE ( 'NONE', *, *, #466, .F. ) ;
#10622 = CARTESIAN_POINT ( 'NONE',  ( 0.5477065543514035850, 0.000000000000000000, -1.934182851860891672 ) ) ;
#10623 = CARTESIAN_POINT ( 'NONE',  ( -61.99999999999998579, 13.76562499965860020, 2.498450539062049724 ) ) ;
#10624 = AXIS2_PLACEMENT_3D ( 'NONE', #8904, #1502, #4878 ) ;
#10625 = CARTESIAN_POINT ( 'NONE',  ( -62.86468353124998032, 9.932291666325268054, 1.000774730468978024 ) ) ;
#10626 = DIRECTION ( 'NONE',  ( 0.000000000000000000, 0.000000000000000000, -1.000000000000000000 ) ) ;
#10627 = ORIENTED_EDGE ( 'NONE', *, *, #9615, .F. ) ;
#10628 = CARTESIAN_POINT ( 'NONE',  ( -61.13531646874997705, 11.66145833299193590, 1.000774730468978468 ) ) ;
#10629 = VECTOR ( 'NONE', #5183, 1000.000000000000000 ) ;
#10630 = CARTESIAN_POINT ( 'NONE',  ( 145.0000000000000284, 5.500000000000000000, 7.300000000000000711 ) ) ;
#10631 = CARTESIAN_POINT ( 'NONE',  ( -61.99999999999998579, 15.06249999999999822, 0.5000000000000013323 ) ) ;
#10632 = CARTESIAN_POINT ( 'NONE',  ( -61.49999999999998579, 14.67708333265053611, 2.366025403784441927 ) ) ;
#10633 = CARTESIAN_POINT ( 'NONE',  ( 140.0000000000000284, -8.000000000000000000, 3.000000000000000000 ) ) ;
#10634 = ORIENTED_EDGE ( 'NONE', *, *, #2980, .T. ) ;
#10635 = CARTESIAN_POINT ( 'NONE',  ( -61.49999999999998579, 15.17708333265053611, 2.366025403784441927 ) ) ;
#10636 = AXIS2_PLACEMENT_3D ( 'NONE', #1149, #4475, #4530 ) ;
#10637 = VERTEX_POINT ( 'NONE', #8293 ) ;
#10638 = PRESENTATION_LAYER_ASSIGNMENT (  '', '', ( #7798 ) ) ;
#10639 = CARTESIAN_POINT ( 'NONE',  ( -61.99999999999999289, 12.51562499965860198, 2.498450539062049724 ) ) ;
#10640 = CARTESIAN_POINT ( 'NONE',  ( -61.56765823437498852, 9.036458332991935904, 2.248837904296538515 ) ) ;
#10641 = CARTESIAN_POINT ( 'NONE',  ( -77.99999999999998579, -11.50000000000000711, 5.000000000000000000 ) ) ;
#10642 = ORIENTED_EDGE ( 'NONE', *, *, #5576, .T. ) ;
#10643 = CARTESIAN_POINT ( 'NONE',  ( -62.99999999999998579, 12.10416666666666430, 0.9226497308103756012 ) ) ;
#10644 = CARTESIAN_POINT ( 'NONE',  ( -62.99999999999998579, 11.09374999931720218, 1.500000000000001998 ) ) ;
#10645 = AXIS2_PLACEMENT_3D ( 'NONE', #8677, #1058, #7570 ) ;
#10646 =( NAMED_UNIT ( * ) PLANE_ANGLE_UNIT ( ) SI_UNIT ( $, .RADIAN. ) );
#10647 = DIRECTION ( 'NONE',  ( 0.000000000000000000, 1.000000000000000000, 0.000000000000000000 ) ) ;
#10648 = EDGE_CURVE ( 'NONE', #484, #1148, #9129, .T. ) ;
#10649 = CARTESIAN_POINT ( 'NONE',  ( -60.99999999999998579, 10.98958333265053611, 0.9226497308103762673 ) ) ;
#10650 =( GEOMETRIC_REPRESENTATION_CONTEXT ( 3 ) GLOBAL_UNCERTAINTY_ASSIGNED_CONTEXT ( ( #7284 ) ) GLOBAL_UNIT_ASSIGNED_CONTEXT ( ( #6966, #850, #7637 ) ) REPRESENTATION_CONTEXT ( 'NONE', 'WORKASPACE' ) );
#10651 = ORIENTED_EDGE ( 'NONE', *, *, #8136, .T. ) ;
#10652 = EDGE_CURVE ( 'NONE', #5305, #2384, #3956, .T. ) ;
#10653 = CARTESIAN_POINT ( 'NONE',  ( -61.99999999999998579, 14.93749999999999822, 2.500000000000002665 ) ) ;
#10654 = CIRCLE ( 'NONE', #8691, 2.000000000000000000 ) ;
#10655 = CARTESIAN_POINT ( 'NONE',  ( -61.13531646874998415, 12.57812499965860198, 1.500000000000002220 ) ) ;
#10656 = EDGE_CURVE ( 'NONE', #6076, #8797, #487, .T. ) ;
#10657 = SURFACE_STYLE_USAGE ( .BOTH. , #8056 ) ;
#10658 = ORIENTED_EDGE ( 'NONE', *, *, #6274, .F. ) ;
#10659 = ORIENTED_EDGE ( 'NONE', *, *, #801, .T. ) ;
#10660 = CARTESIAN_POINT ( 'NONE',  ( -61.56765823437498142, 11.68229166632526805, 0.7511620957034663704 ) ) ;
#10661 = CARTESIAN_POINT ( 'NONE',  ( 0.5000000000000000000, 0.2499999999999982792, 1.911797424705720339 ) ) ;
#10662 = CYLINDRICAL_SURFACE ( 'NONE', #2825, 1.000000000000000888 ) ;
#10663 = EDGE_LOOP ( 'NONE', ( #2665, #6105, #10137, #5819, #9241, #6047 ) ) ;
#10664 = LINE ( 'NONE', #4870, #7109 ) ;
#10665 = EDGE_CURVE ( 'NONE', #2429, #4976, #3385, .T. ) ;
#10666 = ORIENTED_EDGE ( 'NONE', *, *, #7333, .T. ) ;
#10667 = CARTESIAN_POINT ( 'NONE',  ( -62.99999999999998579, 10.35416666666666785, 0.9226497308103756012 ) ) ;
#10668 = CARTESIAN_POINT ( 'NONE',  ( -32.99999999999997158, -14.00000000000000888, 5.000000000000000000 ) ) ;
#10669 = APPLICATION_CONTEXT ( 'automotive_design' ) ;
#10670 = CARTESIAN_POINT ( 'NONE',  ( -61.99999999999998579, 14.53124999931720041, 0.5000000000000013323 ) ) ;
#10671 = DIRECTION ( 'NONE',  ( -0.000000000000000000, -1.000000000000000000, -0.000000000000000000 ) ) ;
#10672 = CARTESIAN_POINT ( 'NONE',  ( -61.49999999999998579, 8.510416665983868256, 0.6339745962155628467 ) ) ;
#10673 = CARTESIAN_POINT ( 'NONE',  ( -62.86468353124998032, 11.74479166632526628, 1.000774730468978246 ) ) ;
#10674 = LINE ( 'NONE', #8735, #743 ) ;
#10675 = ORIENTED_EDGE ( 'NONE', *, *, #497, .F. ) ;
#10676 = EDGE_CURVE ( 'NONE', #5429, #4238, #168, .T. ) ;
#10677 =( BOUNDED_CURVE ( )  B_SPLINE_CURVE ( 2, ( #4075, #7476, #2461, #10022, #2405, #9246, #1633, #10342, #7072, #237, #1005, #8745, #9454, #9508, #8683, #10454, #2792, #6961, #1962, #3621, #1125, #7853, #7797, #1182, #181, #10280, #7742, #5164, #6910, #5220, #2685, #6181, #4507, #6011, #350, #9399, #4559, #3506, #8626, #290, #1793, #3562, #5274, #1851, #5330, #2856, #6122, #6068, #7910, #4386, #3673, #6242, #6851, #2739, #1903, #1064, #4450, #7016, #8573, #8800, #2623, #10395, #9570, #2022, #9628, #5394, #7968, #10221, #952, #4331, #121, #5512, #3853, #7242, #5448, #5678, #10517, #8191, #3075, #7300, #8245, #8915, #577, #8857, #3738, #3962, #9072, #9016, #6473, #10625, #9904, #2193, #6353, #8969, #10740, #1242, #9799, #1303, #2913, #6302, #7189, #3125, #468, #5571, #4625, #1461, #4679, #8087, #3022, #2968, #5621, #9854, #6522, #2241, #2294, #1360, #1409, #9740, #4838, #7134, #4786, #7351, #415, #9683, #2077, #8024, #10685, #3799, #4727, #10571, #2136, #6416, #8137, #525, #3910, #1749, #7029, #190, #10407, #906, #3520, #4235, #77, #9520, #1861, #7642, #10353, #8585, #5288, #9467, #10233, #6975, #7698, #7751, #6920, #8699, #1016, #5174, #3574, #5231, #2750, #6080, #6024, #2807, #9410, #8527, #5965, #3407, #5123, #3462, #4288, #4399, #6136, #27, #9581, #6814, #6194, #6860, #2638, #1915, #10182, #1803, #10291, #962, #1075, #4463, #4340, #131, #7868, #2694, #2579, #8636, #248, #7810, #3632, #5070, #8471, #857, #9353, #5585, #9755, #9643, #8811, #1193, #3687, #4573, #7088, #1138, #7981, #10583, #4520, #10467, #3921, #10639, #7923, #6430, #366, #8757, #3038, #6366, #8099, #5462, #10700, #3750, #3089, #2151, #303, #5523, #7148, #1257, #4637, #9697, #8980, #1372, #5407, #8870, #2868, #10528, #2928, #6257, #540, #9811, #1318, #8927, #6485, #6313, #2089, #1974, #2033, #8039, #428, #3813, #7203, #2981, #4691, #7311, #481, #3866, #7257, #2205, #4742, #8151, #5344, #5635, #2309, #2403, #10952, #3239, #4801, #3341, #6593, #8258, #641, #4073, #6645, #6690, #9086, #10066, #4020, #3294, #7474, #1475, #9244, #9867, #744, #1573, #793, #2459, #593, #5793, #9189, #8299, #1422, #7416, #5849, #10800, #10853, #8202, #3139, #3191, #6536, #4958, #689, #9972, #3977, #8358, #5009, #4851, #2255, #2355, #4128, #7523, #9030, #4172, #5691, #10020, #1630, #10905, #8411, #7572, #5743, #7366, #9137, #10750, #9920, #1526, #4900, #5904, #8458, #8681, #4383, #1685, #177, #5108, #2515, #7795, #119, #1849, #842, #67, #5162, #7850, #3503, #5059, #6907, #8514, #6009, #9397, #3449, #2737, #6120, #10171, #10219, #4224, #894, #2568, #7629, #5270, #2683, #2620, #4275, #235, #5954, #9341, #6744, #14, #6849, #1791, #8571, #6800, #950, #4329, #1062, #7738, #6066, #10278, #9452, #5218, #1901, #8624, #1733, #7684, #1002, #10116, #3560 ),
 .UNSPECIFIED., .F., .T. ) 
 B_SPLINE_CURVE_WITH_KNOTS ( ( 3, 2, 2, 2, 2, 2, 2, 2, 2, 2, 2, 2, 2, 2, 2, 2, 2, 2, 2, 2, 2, 2, 2, 2, 2, 2, 2, 2, 2, 2, 2, 2, 2, 2, 2, 2, 2, 2, 2, 2, 2, 2, 2, 2, 2, 2, 2, 2, 2, 2, 2, 2, 2, 2, 2, 2, 2, 2, 2, 2, 2, 2, 2, 2, 2, 2, 2, 2, 2, 2, 2, 2, 2, 2, 2, 2, 2, 2, 2, 2, 2, 2, 2, 2, 2, 2, 2, 2, 2, 2, 2, 2, 2, 2, 2, 2, 2, 2, 2, 2, 2, 2, 2, 2, 2, 2, 2, 2, 2, 2, 2, 2, 2, 2, 2, 2, 2, 2, 2, 2, 2, 2, 2, 2, 2, 2, 2, 2, 2, 2, 2, 2, 2, 2, 2, 2, 2, 2, 2, 2, 2, 2, 2, 2, 2, 2, 2, 2, 2, 2, 2, 2, 2, 2, 2, 2, 2, 2, 2, 2, 2, 2, 2, 2, 2, 2, 2, 2, 2, 2, 2, 2, 2, 2, 2, 2, 2, 2, 2, 2, 2, 2, 2, 2, 2, 2, 2, 2, 2, 2, 2, 2, 3 ),
 ( 0.000000000000000000, 0.005208333333333333044, 0.01041666666666666609, 0.01562500000000000000, 0.02083333333333333218, 0.02604166666666666782, 0.03125000000000000000, 0.03645833333333333565, 0.04166666666666666435, 0.04687500000000000000, 0.05208333333333333565, 0.05729166666666666435, 0.06250000000000000000, 0.06770833333333332871, 0.07291666666666667129, 0.07812500000000000000, 0.08333333333333332871, 0.08854166666666667129, 0.09375000000000000000, 0.09895833333333332871, 0.1041666666666666713, 0.1093750000000000000, 0.1145833333333333287, 0.1197916666666666713, 0.1250000000000000000, 0.1302083333333333426, 0.1354166666666666574, 0.1406250000000000000, 0.1458333333333333426, 0.1510416666666666574, 0.1562500000000000000, 0.1614583333333333426, 0.1666666666666666574, 0.1718750000000000000, 0.1770833333333333426, 0.1822916666666666574, 0.1875000000000000000, 0.1927083333333333426, 0.1979166666666666574, 0.2031250000000000000, 0.2083333333333333426, 0.2135416666666666574, 0.2187500000000000000, 0.2239583333333333426, 0.2291666666666666574, 0.2343750000000000000, 0.2395833333333333426, 0.2447916666666666574, 0.2500000000000000000, 0.2552083333333333148, 0.2604166666666666852, 0.2656250000000000000, 0.2708333333333333148, 0.2760416666666666852, 0.2812500000000000000, 0.2864583333333333148, 0.2916666666666666852, 0.2968750000000000000, 0.3020833333333333148, 0.3072916666666666852, 0.3125000000000000000, 0.3177083333333333148, 0.3229166666666666852, 0.3281250000000000000, 0.3333333333333333148, 0.3385416666666666852, 0.3437500000000000000, 0.3489583333333333148, 0.3541666666666666852, 0.3593750000000000000, 0.3645833333333333148, 0.3697916666666666852, 0.3750000000000000000, 0.3802083333333333148, 0.3854166666666666852, 0.3906250000000000000, 0.3958333333333333148, 0.4010416666666666852, 0.4062500000000000000, 0.4114583333333333148, 0.4166666666666666852, 0.4218750000000000000, 0.4270833333333333148, 0.4322916666666666852, 0.4375000000000000000, 0.4427083333333333148, 0.4479166666666666852, 0.4531250000000000000, 0.4583333333333333148, 0.4635416666666666852, 0.4687500000000000000, 0.4739583333333333148, 0.4791666666666666852, 0.4843750000000000000, 0.4895833333333333148, 0.4947916666666666852, 0.5000000000000000000, 0.5052083333333333703, 0.5104166666666666297, 0.5156250000000000000, 0.5208333333333333703, 0.5260416666666666297, 0.5312500000000000000, 0.5364583333333333703, 0.5416666666666666297, 0.5468750000000000000, 0.5520833333333333703, 0.5572916666666666297, 0.5625000000000000000, 0.5677083333333333703, 0.5729166666666666297, 0.5781250000000000000, 0.5833333333333333703, 0.5885416666666666297, 0.5937500000000000000, 0.5989583333333333703, 0.6041666666666666297, 0.6093750000000000000, 0.6145833333333333703, 0.6197916666666666297, 0.6250000000000000000, 0.6302083333333333703, 0.6354166666666666297, 0.6406250000000000000, 0.6458333333333333703, 0.6510416666666666297, 0.6562500000000000000, 0.6614583333333333703, 0.6666666666666666297, 0.6718750000000000000, 0.6770833333333333703, 0.6822916666666666297, 0.6875000000000000000, 0.6927083333333333703, 0.6979166666666666297, 0.7031250000000000000, 0.7083333333333333703, 0.7135416666666666297, 0.7187500000000000000, 0.7239583333333333703, 0.7291666666666666297, 0.7343750000000000000, 0.7395833333333333703, 0.7447916666666666297, 0.7500000000000000000, 0.7552083333333333703, 0.7604166666666666297, 0.7656250000000000000, 0.7708333333333333703, 0.7760416666666666297, 0.7812500000000000000, 0.7864583333333333703, 0.7916666666666666297, 0.7968750000000000000, 0.8020833333333333703, 0.8072916666666666297, 0.8125000000000000000, 0.8177083333333333703, 0.8229166666666666297, 0.8281250000000000000, 0.8333333333333333703, 0.8385416666666666297, 0.8437500000000000000, 0.8489583333333333703, 0.8541666666666666297, 0.8593750000000000000, 0.8645833333333333703, 0.8697916666666666297, 0.8750000000000000000, 0.8802083333333333703, 0.8854166666666666297, 0.8906250000000000000, 0.8958333333333333703, 0.9010416666666666297, 0.9062500000000000000, 0.9114583333333333703, 0.9166666666666666297, 0.9218750000000000000, 0.9270833333333333703, 0.9322916666666666297, 0.9375000000000000000, 0.9427083333333333703, 0.9479166666666666297, 0.9531250000000000000, 0.9583333333333333703, 0.9635416666666666297, 0.9687500000000000000, 0.9739583333333333703, 0.9791666666666666297, 0.9843750000000000000, 0.9895833333333333703, 0.9947916666666666297, 1.000000000000000000 ),
 .UNSPECIFIED. ) 
 CURVE ( )  GEOMETRIC_REPRESENTATION_ITEM ( )  RATIONAL_B_SPLINE_CURVE ( ( 1.000000000000000000, 0.8660254037844387076, 1.000000000000000000, 0.8660254037844387076, 1.000000000000000000, 0.8660254037844387076, 1.000000000000000000, 0.8660254037844387076, 1.000000000000000000, 0.8660254037844387076, 1.000000000000000000, 0.8660254037844387076, 1.000000000000000000, 0.8660254037844387076, 1.000000000000000000, 0.8660254037844387076, 1.000000000000000000, 0.8660254037844387076, 1.000000000000000000, 0.8660254037844387076, 1.000000000000000000, 0.8660254037844387076, 1.000000000000000000, 0.8660254037844387076, 1.000000000000000000, 0.8660254037844387076, 1.000000000000000000, 0.8660254037844387076, 1.000000000000000000, 0.8660254037844387076, 1.000000000000000000, 0.8660254037844387076, 1.000000000000000000, 0.8660254037844387076, 1.000000000000000000, 0.8660254037844387076, 1.000000000000000000, 0.8660254037844387076, 1.000000000000000000, 0.8660254037844387076, 1.000000000000000000, 0.8660254037844387076, 1.000000000000000000, 0.8660254037844387076, 1.000000000000000000, 0.8660254037844387076, 1.000000000000000000, 0.8660254037844387076, 1.000000000000000000, 0.8660254037844387076, 1.000000000000000000, 0.8660254037844387076, 1.000000000000000000, 0.8660254037844387076, 1.000000000000000000, 0.8660254037844387076, 1.000000000000000000, 0.8660254037844387076, 1.000000000000000000, 0.8660254037844387076, 1.000000000000000000, 0.8660254037844387076, 1.000000000000000000, 0.8660254037844387076, 1.000000000000000000, 0.8660254037844387076, 1.000000000000000000, 0.8660254037844387076, 1.000000000000000000, 0.8660254037844387076, 1.000000000000000000, 0.8660254037844387076, 1.000000000000000000, 0.8660254037844387076, 1.000000000000000000, 0.8660254037844387076, 1.000000000000000000, 0.8660254037844387076, 1.000000000000000000, 0.8660254037844387076, 1.000000000000000000, 0.8660254037844387076, 1.000000000000000000, 0.8660254037844387076, 1.000000000000000000, 0.8660254037844387076, 1.000000000000000000, 0.8660254037844387076, 1.000000000000000000, 0.8660254037844387076, 1.000000000000000000, 0.8660254037844387076, 1.000000000000000000, 0.8660254037844387076, 1.000000000000000000, 0.8660254037844387076, 1.000000000000000000, 0.8660254037844387076, 1.000000000000000000, 0.8660254037844387076, 1.000000000000000000, 0.8660254037844387076, 1.000000000000000000, 0.8660254037844387076, 1.000000000000000000, 0.8660254037844387076, 1.000000000000000000, 0.8660254037844387076, 1.000000000000000000, 0.8660254037844387076, 1.000000000000000000, 0.8660254037844387076, 1.000000000000000000, 0.8660254037844387076, 1.000000000000000000, 0.8660254037844387076, 1.000000000000000000, 0.8660254037844387076, 1.000000000000000000, 0.8660254037844387076, 1.000000000000000000, 0.8660254037844387076, 1.000000000000000000, 0.8660254037844387076, 1.000000000000000000, 0.8660254037844387076, 1.000000000000000000, 0.8660254037844387076, 1.000000000000000000, 0.8660254037844387076, 1.000000000000000000, 0.8660254037844387076, 1.000000000000000000, 0.8660254037844387076, 1.000000000000000000, 0.8660254037844387076, 1.000000000000000000, 0.8660254037844387076, 1.000000000000000000, 0.8660254037844387076, 1.000000000000000000, 0.8660254037844387076, 1.000000000000000000, 0.8660254037844387076, 1.000000000000000000, 0.8660254037844387076, 1.000000000000000000, 0.8660254037844387076, 1.000000000000000000, 0.8660254037844387076, 1.000000000000000000, 0.8660254037844387076, 1.000000000000000000, 0.8660254037844387076, 1.000000000000000000, 0.8660254037844387076, 1.000000000000000000, 0.8660254037844387076, 1.000000000000000000, 0.8660254037844387076, 1.000000000000000000, 0.8660254037844387076, 1.000000000000000000, 0.8660254037844387076, 1.000000000000000000, 0.8660254037844387076, 1.000000000000000000, 0.8660254037844387076, 1.000000000000000000, 0.8660254037844387076, 1.000000000000000000, 0.8660254037844387076, 1.000000000000000000, 0.8660254037844387076, 1.000000000000000000, 0.8660254037844387076, 1.000000000000000000, 0.8660254037844387076, 1.000000000000000000, 0.8660254037844387076, 1.000000000000000000, 0.8660254037844387076, 1.000000000000000000, 0.8660254037844387076, 1.000000000000000000, 0.8660254037844387076, 1.000000000000000000, 0.8660254037844387076, 1.000000000000000000, 0.8660254037844387076, 1.000000000000000000, 0.8660254037844387076, 1.000000000000000000, 0.8660254037844387076, 1.000000000000000000, 0.8660254037844387076, 1.000000000000000000, 0.8660254037844387076, 1.000000000000000000, 0.8660254037844387076, 1.000000000000000000, 0.8660254037844387076, 1.000000000000000000, 0.8660254037844387076, 1.000000000000000000, 0.8660254037844387076, 1.000000000000000000, 0.8660254037844387076, 1.000000000000000000, 0.8660254037844387076, 1.000000000000000000, 0.8660254037844387076, 1.000000000000000000, 0.8660254037844387076, 1.000000000000000000, 0.8660254037844387076, 1.000000000000000000, 0.8660254037844387076, 1.000000000000000000, 0.8660254037844387076, 1.000000000000000000, 0.8660254037844387076, 1.000000000000000000, 0.8660254037844387076, 1.000000000000000000, 0.8660254037844387076, 1.000000000000000000, 0.8660254037844387076, 1.000000000000000000, 0.8660254037844387076, 1.000000000000000000, 0.8660254037844387076, 1.000000000000000000, 0.8660254037844387076, 1.000000000000000000, 0.8660254037844387076, 1.000000000000000000, 0.8660254037844387076, 1.000000000000000000, 0.8660254037844387076, 1.000000000000000000, 0.8660254037844387076, 1.000000000000000000, 0.8660254037844387076, 1.000000000000000000, 0.8660254037844387076, 1.000000000000000000, 0.8660254037844387076, 1.000000000000000000, 0.8660254037844387076, 1.000000000000000000, 0.8660254037844387076, 1.000000000000000000, 0.8660254037844387076, 1.000000000000000000, 0.8660254037844387076, 1.000000000000000000, 0.8660254037844387076, 1.000000000000000000, 0.8660254037844387076, 1.000000000000000000, 0.8660254037844387076, 1.000000000000000000, 0.8660254037844387076, 1.000000000000000000, 0.8660254037844387076, 1.000000000000000000, 0.8660254037844387076, 1.000000000000000000, 0.8660254037844387076, 1.000000000000000000, 0.8660254037844387076, 1.000000000000000000, 0.8660254037844387076, 1.000000000000000000, 0.8660254037844387076, 1.000000000000000000, 0.8660254037844387076, 1.000000000000000000, 0.8660254037844387076, 1.000000000000000000, 0.8660254037844387076, 1.000000000000000000, 0.8660254037844387076, 1.000000000000000000, 0.8660254037844387076, 1.000000000000000000, 0.8660254037844387076, 1.000000000000000000, 0.8660254037844387076, 1.000000000000000000, 0.8660254037844387076, 1.000000000000000000, 0.8660254037844387076, 1.000000000000000000, 0.8660254037844387076, 1.000000000000000000, 0.8660254037844387076, 1.000000000000000000, 0.8660254037844387076, 1.000000000000000000, 0.8660254037844387076, 1.000000000000000000, 0.8660254037844387076, 1.000000000000000000, 0.8660254037844387076, 1.000000000000000000, 0.8660254037844387076, 1.000000000000000000, 0.8660254037844387076, 1.000000000000000000, 0.8660254037844387076, 1.000000000000000000, 0.8660254037844387076, 1.000000000000000000, 0.8660254037844387076, 1.000000000000000000, 0.8660254037844387076, 1.000000000000000000, 0.8660254037844387076, 1.000000000000000000, 0.8660254037844387076, 1.000000000000000000, 0.8660254037844387076, 1.000000000000000000, 0.8660254037844387076, 1.000000000000000000, 0.8660254037844387076, 1.000000000000000000, 0.8660254037844387076, 1.000000000000000000, 0.8660254037844387076, 1.000000000000000000, 0.8660254037844387076, 1.000000000000000000, 0.8660254037844387076, 1.000000000000000000, 0.8660254037844387076, 1.000000000000000000, 0.8660254037844387076, 1.000000000000000000, 0.8660254037844387076, 1.000000000000000000, 0.8660254037844387076, 1.000000000000000000, 0.8660254037844387076, 1.000000000000000000, 0.8660254037844387076, 1.000000000000000000, 0.8660254037844387076, 1.000000000000000000, 0.8660254037844387076, 1.000000000000000000, 0.8660254037844387076, 1.000000000000000000, 0.8660254037844387076, 1.000000000000000000, 0.8660254037844387076, 1.000000000000000000, 0.8660254037844387076, 1.000000000000000000, 0.8660254037844387076, 1.000000000000000000, 0.8660254037844387076, 1.000000000000000000, 0.8660254037844387076, 1.000000000000000000, 0.8660254037844387076, 1.000000000000000000, 0.8660254037844387076, 1.000000000000000000, 0.8660254037844387076, 1.000000000000000000, 0.8660254037844387076, 1.000000000000000000, 0.8660254037844387076, 1.000000000000000000, 0.8660254037844387076, 1.000000000000000000, 0.8660254037844387076, 1.000000000000000000, 0.8660254037844387076, 1.000000000000000000, 0.8660254037844387076, 1.000000000000000000 ) ) 
 REPRESENTATION_ITEM ( '' )  );
#10678 = AXIS2_PLACEMENT_3D ( 'NONE', #4278, #846, #7854 ) ;
#10679 = DIRECTION ( 'NONE',  ( -0.000000000000000000, -0.000000000000000000, -1.000000000000000000 ) ) ;
#10680 = DIRECTION ( 'NONE',  ( 0.000000000000000000, 0.000000000000000000, 1.000000000000000000 ) ) ;
#10681 = EDGE_CURVE ( 'NONE', #3104, #3152, #10162, .T. ) ;
#10682 = ORIENTED_EDGE ( 'NONE', *, *, #572, .F. ) ;
#10683 = DIRECTION ( 'NONE',  ( -0.000000000000000000, -0.000000000000000000, -1.000000000000000000 ) ) ;
#10684 = CARTESIAN_POINT ( 'NONE',  ( -61.13531646874998415, 13.30729166632526983, 1.999225269531026417 ) ) ;
#10685 = CARTESIAN_POINT ( 'NONE',  ( -62.86468353124999453, 10.70312499965860020, 1.500000000000002220 ) ) ;
#10686 = LINE ( 'NONE', #8858, #4757 ) ;
#10687 = VERTEX_POINT ( 'NONE', #8450 ) ;
#10688 = CARTESIAN_POINT ( 'NONE',  ( -61.99999999999998579, 16.00000000000000000, 0.5000000000000041078 ) ) ;
#10689 = CARTESIAN_POINT ( 'NONE',  ( -61.99999999999999289, 11.32812499965860020, 2.498450539062049724 ) ) ;
#10690 = PRODUCT_CONTEXT ( 'NONE', #4975, 'mechanical' ) ;
#10691 = FACE_OUTER_BOUND ( 'NONE', #10201, .T. ) ;
#10692 = EDGE_CURVE ( 'NONE', #6498, #7723, #4267, .T. ) ;
#10693 = CARTESIAN_POINT ( 'NONE',  ( -61.99999999999998579, 8.203124999658601979, 0.5015494609379544944 ) ) ;
#10694 = DIRECTION ( 'NONE',  ( 0.000000000000000000, 0.000000000000000000, -1.000000000000000000 ) ) ;
#10695 = ORIENTED_EDGE ( 'NONE', *, *, #1280, .T. ) ;
#10696 = CARTESIAN_POINT ( 'NONE',  ( -61.73205080756886076, 15.27008544963257108, 0.5000000000000014433 ) ) ;
#10697 = EDGE_LOOP ( 'NONE', ( #6533, #6428, #9662, #1033 ) ) ;
#10698 = AXIS2_PLACEMENT_3D ( 'NONE', #6293, #10563, #1294 ) ;
#10699 = VECTOR ( 'NONE', #6675, 1000.000000000000000 ) ;
#10700 = CARTESIAN_POINT ( 'NONE',  ( -62.86468353124999453, 12.70312499965860198, 1.500000000000002220 ) ) ;
#10701 = CARTESIAN_POINT ( 'NONE',  ( -62.86468353124999453, 9.953124999658601979, 1.500000000000002220 ) ) ;
#10702 = DIRECTION ( 'NONE',  ( -0.000000000000000000, -0.000000000000000000, -1.000000000000000000 ) ) ;
#10703 = ORIENTED_EDGE ( 'NONE', *, *, #97, .T. ) ;
#10704 = CARTESIAN_POINT ( 'NONE',  ( -62.99999999999998579, 14.10416666666666607, 0.9226497308103756012 ) ) ;
#10705 = CARTESIAN_POINT ( 'NONE',  ( -61.99999999999998579, 16.00000000000000000, 1.500000000000002220 ) ) ;
#10706 =( LENGTH_UNIT ( ) NAMED_UNIT ( * ) SI_UNIT ( .MILLI., .METRE. ) );
#10707 = UNCERTAINTY_MEASURE_WITH_UNIT (LENGTH_MEASURE( 1.000000000000000082E-05 ), #8264, 'distance_accuracy_value', 'NONE');
#10708 = AXIS2_PLACEMENT_3D ( 'NONE', #7978, #5404, #2086 ) ;
#10709 = VECTOR ( 'NONE', #4465, 1000.000000000000000 ) ;
#10710 = CARTESIAN_POINT ( 'NONE',  ( -62.99999999999998579, 12.59374999931720396, 1.500000000000001998 ) ) ;
#10711 = CARTESIAN_POINT ( 'NONE',  ( 0.000000000000000000, -0.2500000000000001110, 1.312875263449798879 ) ) ;
#10712 = VECTOR ( 'NONE', #9691, 1000.000000000000000 ) ;
#10713 = CARTESIAN_POINT ( 'NONE',  ( -61.99999999999998579, 12.39062499965860198, 0.5015494609379544944 ) ) ;
#10714 = ADVANCED_FACE ( 'NONE', ( #3553 ), #1783, .T. ) ;
#10715 = CARTESIAN_POINT ( 'NONE',  ( -60.99999999999998579, 11.52083333333333393, 0.9226497308103762673 ) ) ;
#10716 = ORIENTED_EDGE ( 'NONE', *, *, #10676, .T. ) ;
#10717 = ADVANCED_FACE ( 'NONE', ( #7620 ), #9286, .T. ) ;
#10718 = CARTESIAN_POINT ( 'NONE',  ( -61.56765823437498852, 11.09895833299193590, 2.248837904296538515 ) ) ;
#10719 = CARTESIAN_POINT ( 'NONE',  ( -61.99999999999998579, -8.000000000000000000, 1.500000000000002220 ) ) ;
#10720 = AXIS2_PLACEMENT_3D ( 'NONE', #10186, #9061, #8425 ) ;
#10721 = CARTESIAN_POINT ( 'NONE',  ( -61.99999999999998579, 10.90624999931720218, 2.500000000000002665 ) ) ;
#10722 = ORIENTED_EDGE ( 'NONE', *, *, #2597, .T. ) ;
#10723 = CARTESIAN_POINT ( 'NONE',  ( -62.99999999999998579, 11.12500000000000000, 1.500000000000001998 ) ) ;
#10724 = ORIENTED_EDGE ( 'NONE', *, *, #10570, .T. ) ;
#10725 = PLANE ( 'NONE',  #8227 ) ;
#10726 = CARTESIAN_POINT ( 'NONE',  ( -62.99999999999998579, 10.39583333333333215, 2.077350269189627952 ) ) ;
#10727 = CARTESIAN_POINT ( 'NONE',  ( -61.73205080756886076, 11.19866454968462754, 2.500000000000003109 ) ) ;
#10728 = FACE_OUTER_BOUND ( 'NONE', #6832, .T. ) ;
#10729 = CARTESIAN_POINT ( 'NONE',  ( -61.99999999999998579, 12.18749999999999822, 2.500000000000002665 ) ) ;
#10730 = CARTESIAN_POINT ( 'NONE',  ( -77.99999999999998579, 0.000000000000000000, 10.99999999999999289 ) ) ;
#10731 = EDGE_CURVE ( 'NONE', #2188, #5900, #1725, .T. ) ;
#10732 = CARTESIAN_POINT ( 'NONE',  ( -62.86468353124998742, 11.78645833299193590, 1.999225269531025972 ) ) ;
#10733 = DIRECTION ( 'NONE',  ( -1.000000000000000000, -0.000000000000000000, -0.000000000000000000 ) ) ;
#10734 = VERTEX_POINT ( 'NONE', #6897 ) ;
#10735 = DIRECTION ( 'NONE',  ( 1.110223024625156343E-15, 1.000000000000000000, -0.000000000000000000 ) ) ;
#10736 = LINE ( 'NONE', #5672, #8580 ) ;
#10737 = ORIENTED_EDGE ( 'NONE', *, *, #8905, .T. ) ;
#10738 = LINE ( 'NONE', #3959, #6447 ) ;
#10739 = CARTESIAN_POINT ( 'NONE',  ( -61.13531646874998415, 13.34895833299193413, 1.000774730468978468 ) ) ;
#10740 = CARTESIAN_POINT ( 'NONE',  ( -61.56765823437498852, 10.03645833299193413, 2.248837904296538515 ) ) ;
#10741 = FILL_AREA_STYLE_COLOUR ( '', #514 ) ;
#10742 = ORIENTED_EDGE ( 'NONE', *, *, #6052, .F. ) ;
#10743 = CARTESIAN_POINT ( 'NONE',  ( -62.86468353124999453, 11.26562499965860020, 1.500000000000002220 ) ) ;
#10744 = CARTESIAN_POINT ( 'NONE',  ( -62.86468353124999453, 16.01562499965860198, 1.500000000000002220 ) ) ;
#10745 = CARTESIAN_POINT ( 'NONE',  ( -62.99999999999998579, 16.11458333265053255, 2.077350269189627952 ) ) ;
#10746 = DIRECTION ( 'NONE',  ( -1.000000000000000000, 0.000000000000000000, -0.000000000000000000 ) ) ;
#10747 = ORIENTED_EDGE ( 'NONE', *, *, #3784, .T. ) ;
#10748 = FACE_BOUND ( 'NONE', #10228, .T. ) ;
#10749 = DIRECTION ( 'NONE',  ( 0.000000000000000000, -1.000000000000000000, 0.000000000000000000 ) ) ;
#10750 = CARTESIAN_POINT ( 'NONE',  ( -61.13531646874997705, 14.80729166632526805, 1.999225269531026417 ) ) ;
#10751 = CARTESIAN_POINT ( 'NONE',  ( -62.43234176562499016, 9.744791666325268054, 2.248837904296538071 ) ) ;
#10752 = DIRECTION ( 'NONE',  ( 0.000000000000000000, 0.000000000000000000, 1.000000000000000000 ) ) ;
#10753 = ORIENTED_EDGE ( 'NONE', *, *, #6274, .T. ) ;
#10754 = CARTESIAN_POINT ( 'NONE',  ( -61.99999999999998579, 14.31250000000000000, 0.3452994616207497591 ) ) ;
#10755 = CARTESIAN_POINT ( 'NONE',  ( -62.49999999999998579, 8.552083332650536107, 0.6339745962155627357 ) ) ;
#10756 = CARTESIAN_POINT ( 'NONE',  ( -61.99999999999998579, 12.03124999931720218, 0.3452994616207497591 ) ) ;
#10757 = CARTESIAN_POINT ( 'NONE',  ( -61.99999999999998579, 12.28124999931720041, 0.5000000000000013323 ) ) ;
#10758 = CARTESIAN_POINT ( 'NONE',  ( -61.13531646874998415, 14.34895833299193413, 1.000774730468978468 ) ) ;
#10759 = ADVANCED_FACE ( 'NONE', ( #7677 ), #9333, .T. ) ;
#10760 = DIRECTION ( 'NONE',  ( 1.000000000000000000, 0.000000000000000000, 0.000000000000000000 ) ) ;
#10761 = ORIENTED_EDGE ( 'NONE', *, *, #107, .F. ) ;
#10762 = CARTESIAN_POINT ( 'NONE',  ( -61.13531646874998415, 12.16145833299193413, 1.000774730468978468 ) ) ;
#10763 = CARTESIAN_POINT ( 'NONE',  ( -149.9999999999999716, 8.000000000000000000, 3.000000000000000000 ) ) ;
#10764 = CARTESIAN_POINT ( 'NONE',  ( -61.13531646874998415, 15.39062499965860020, 1.500000000000002220 ) ) ;
#10765 = ORIENTED_EDGE ( 'NONE', *, *, #7061, .T. ) ;
#10766 = FACE_OUTER_BOUND ( 'NONE', #3378, .T. ) ;
#10767 = EDGE_CURVE ( 'NONE', #8768, #3366, #3495, .T. ) ;
#10768 = EDGE_LOOP ( 'NONE', ( #7506, #9299, #3069, #7543 ) ) ;
#10769 = CARTESIAN_POINT ( 'NONE',  ( -109.9999999999999289, 33.00000000000000711, -2.000000000000000000 ) ) ;
#10770 = CARTESIAN_POINT ( 'NONE',  ( -60.99999999999998579, 9.270833333333333925, 0.9226497308103762673 ) ) ;
#10771 = CARTESIAN_POINT ( 'NONE',  ( -62.99999999999998579, 12.85416666666666607, 0.9226497308103756012 ) ) ;
#10772 = FACE_OUTER_BOUND ( 'NONE', #6361, .T. ) ;
#10773 = CARTESIAN_POINT ( 'NONE',  ( -61.99999999999998579, 12.31249999999999822, 0.5000000000000013323 ) ) ;
#10774 = DIRECTION ( 'NONE',  ( 0.000000000000000000, 0.000000000000000000, -1.000000000000000000 ) ) ;
#10775 = CARTESIAN_POINT ( 'NONE',  ( -61.56765823437498852, 11.59895833299193590, 2.248837904296538515 ) ) ;
#10776 = DIRECTION ( 'NONE',  ( 0.000000000000000000, 0.000000000000000000, -1.000000000000000000 ) ) ;
#10777 = ORIENTED_EDGE ( 'NONE', *, *, #535, .F. ) ;
#10778 = CARTESIAN_POINT ( 'NONE',  ( -60.99999999999998579, 9.197916665983870033, 2.077350269189628840 ) ) ;
#10779 = CIRCLE ( 'NONE', #4197, 1.336466033005844434 ) ;
#10780 = ADVANCED_FACE ( 'NONE', ( #8562 ), #5100, .T. ) ;
#10781 = DIRECTION ( 'NONE',  ( 1.000000000000000000, 0.000000000000000000, 0.000000000000000000 ) ) ;
#10782 = CARTESIAN_POINT ( 'NONE',  ( -61.99999999999998579, 13.78124999931720218, 0.5000000000000013323 ) ) ;
#10783 = EDGE_CURVE ( 'NONE', #9337, #1260, #3896, .T. ) ;
#10784 = CARTESIAN_POINT ( 'NONE',  ( -61.13531646874998415, 13.82812499965860198, 1.500000000000002220 ) ) ;
#10785 = DIRECTION ( 'NONE',  ( 1.000000000000000000, 0.000000000000000000, 0.000000000000000000 ) ) ;
#10786 = CARTESIAN_POINT ( 'NONE',  ( -62.99999999999998579, 8.145833333333333925, 2.077350269189627952 ) ) ;
#10787 = CARTESIAN_POINT ( 'NONE',  ( -62.49999999999998579, 8.302083332650536107, 0.6339745962155627357 ) ) ;
#10788 = CARTESIAN_POINT ( 'NONE',  ( -62.43234176562499016, 11.05729166632526805, 2.248837904296538071 ) ) ;
#10789 = CIRCLE ( 'NONE', #678, 1.000000000000000888 ) ;
#10790 = CARTESIAN_POINT ( 'NONE',  ( -61.99999999999998579, 15.57812499965860198, 2.498450539062049724 ) ) ;
#10791 = PRODUCT_DEFINITION ( 'UNKNOWN', '', #176, #2481 ) ;
#10792 = CARTESIAN_POINT ( 'NONE',  ( -61.99999999999998579, 13.53124999931720041, 0.5000000000000013323 ) ) ;
#10793 = CARTESIAN_POINT ( 'NONE',  ( -62.99999999999998579, 15.34374999931720218, 1.500000000000001998 ) ) ;
#10794 = VECTOR ( 'NONE', #5435, 1000.000000000000000 ) ;
#10795 = CARTESIAN_POINT ( 'NONE',  ( -25.39999999999996305, 0.000000000000000000, 0.000000000000000000 ) ) ;
#10796 = ORIENTED_EDGE ( 'NONE', *, *, #646, .T. ) ;
#10797 = DIRECTION ( 'NONE',  ( -1.000000000000000000, 0.000000000000000000, -0.000000000000000000 ) ) ;
#10798 = CARTESIAN_POINT ( 'NONE',  ( -62.99999999999998579, 12.62500000000000000, 1.500000000000001998 ) ) ;
#10799 = VECTOR ( 'NONE', #333, 1000.000000000000000 ) ;
#10800 = CARTESIAN_POINT ( 'NONE',  ( -62.86468353124999453, 14.22395833299193590, 1.999225269531025750 ) ) ;
#10801 = CARTESIAN_POINT ( 'NONE',  ( -62.86468353124998742, 9.473958332991934128, 1.999225269531025972 ) ) ;
#10802 = AXIS2_PLACEMENT_3D ( 'NONE', #9763, #5735, #4064 ) ;
#10803 = DIRECTION ( 'NONE',  ( -3.469446951953572774E-16, 1.000000000000000000, 0.000000000000000000 ) ) ;
#10804 = EDGE_LOOP ( 'NONE', ( #4817, #8651, #8525, #1822, #9730, #816 ) ) ;
#10805 = CARTESIAN_POINT ( 'NONE',  ( -61.49999999999998579, 13.45833333333333215, 2.366025403784441927 ) ) ;
#10806 = CARTESIAN_POINT ( 'NONE',  ( -62.99999999999998579, 8.572916665983868256, 0.9226497308103756012 ) ) ;
#10807 = AXIS2_PLACEMENT_3D ( 'NONE', #7678, #3332, #6683 ) ;
#10808 = CARTESIAN_POINT ( 'NONE',  ( -60.99999999999998579, 12.19791666598386826, 2.077350269189628840 ) ) ;
#10809 = DIRECTION ( 'NONE',  ( -1.000000000000000000, 0.000000000000000000, 0.000000000000000000 ) ) ;
#10810 = CARTESIAN_POINT ( 'NONE',  ( -61.56765823437498142, 14.11979166632526805, 0.7511620957034663704 ) ) ;
#10811 = FACE_OUTER_BOUND ( 'NONE', #9856, .T. ) ;
#10812 = VECTOR ( 'NONE', #6005, 1000.000000000000000 ) ;
#10813 = EDGE_CURVE ( 'NONE', #7749, #3994, #5155, .T. ) ;
#10814 = EDGE_LOOP ( 'NONE', ( #10975, #9324 ) ) ;
#10815 = MECHANICAL_DESIGN_GEOMETRIC_PRESENTATION_REPRESENTATION (  '', ( #1765 ), #6206 ) ;
#10816 = CARTESIAN_POINT ( 'NONE',  ( -62.86468353124998032, 11.99479166632526805, 1.000774730468978246 ) ) ;
#10817 = DIRECTION ( 'NONE',  ( -0.000000000000000000, -1.000000000000000000, -0.000000000000000000 ) ) ;
#10818 = ADVANCED_FACE ( 'NONE', ( #6735 ), #5050, .T. ) ;
#10819 = CONICAL_SURFACE ( 'NONE', #1427, 23.99999999999999289, 0.7853981633974466137 ) ;
#10820 = CARTESIAN_POINT ( 'NONE',  ( -49.99999999999998579, -15.00000000000001243, 3.000000000000002665 ) ) ;
#10821 = VERTEX_POINT ( 'NONE', #5999 ) ;
#10822 = FACE_OUTER_BOUND ( 'NONE', #5721, .T. ) ;
#10823 = STYLED_ITEM ( 'NONE', ( #6652 ), #10920 ) ;
#10824 = ORIENTED_EDGE ( 'NONE', *, *, #3592, .T. ) ;
#10825 = DIRECTION ( 'NONE',  ( 1.000000000000000000, -1.110223024625156343E-15, 0.000000000000000000 ) ) ;
#10826 = CARTESIAN_POINT ( 'NONE',  ( -62.99999999999998579, 9.625000000000000000, 1.500000000000001998 ) ) ;
#10827 = CARTESIAN_POINT ( 'NONE',  ( -61.49999999999998579, 15.01041666598386826, 0.6339745962155628467 ) ) ;
#10828 = CARTESIAN_POINT ( 'NONE',  ( -61.99999999999997868, 8.312499999999998224, 0.5000000000000013323 ) ) ;
#10829 =( BOUNDED_SURFACE ( )  B_SPLINE_SURFACE ( 1, 2, ( 
 ( #7204, #10584, #9756, #9698, #4692, #1194, #7149, #2809, #1139, #7869, #3814, #2034, #7924, #6367, #2152, #5345, #5524, #5463, #1975, #9812, #6195, #8040, #4574, #3633, #8928, #3751, #304, #1319, #1258, #8100, #9582, #3688, #7030, #2206, #3867, #6314, #10408, #8758, #7982, #8700, #7090, #10468, #2869, #7258, #368, #6258, #10640, #10529, #8871, #4638, #3039, #6431, #1076, #4464, #10067, #9973, #1527, #3192, #3240, #5586, #7312, #8152, #1476, #4901, #2404, #2310, #9921, #10801, #9138, #8981, #7524, #10854, #541, #8360, #4743, #8300, #6646, #5794, #6487, #4852, #10751, #8259, #9868, #745, #4129, #2256, #9190, #4074, #7475, #690, #10701, #5636, #10021, #10906, #9087, #3922, #5692, #1574, #1423, #594, #6537, #4959, #3295, #642, #6691, #1373, #9031, #3090, #4802, #8203, #3978, #2356, #7367, #3140, #4022, #7417, #6594, #5744, #8459, #951, #7685, #4330, #8625, #9398, #3451, #1792, #1735, #2684, #68, #9245, #7630, #1686, #7740, #8572, #2569, #10220, #2621, #120, #4276, #4173, #9453, #7573, #3504, #5163, #5109, #2516, #3561, #15, #2460, #6908, #10279, #6850, #7796, #3393, #5906, #9296, #6067, #5219, #1850, #6010, #6801, #4384, #1004, #178, #5955, #9342, #6959, #5850, #1632, #5060, #843, #8515, #5010, #3342, #10173, #10953, #8412, #794, #6745, #10117, #4225, #895, #3798, #10515, #3737, #8086, #6179, #3620, #6352, #5272, #7188, #467, #10569, #7133, #2967, #289, #7015, #1902, #1961, #4558, #9738, #1063, #8682, #10394, #2912, #7966, #2791, #6300, #3851, #9682, #9569, #4448, #8799, #7909, #1124, #349, #2076, #2135, #5329, #8742, #7851, #5510, #5447, #8855, #10341, #4506, #2738, #10453, #3672, #413, #6121, #1241, #8914, #9507, #1302, #4678, #7070, #2855, #236, #6241, #9627, #2020, #5393, #1181, #4624, #8023, #5570, #4837, #5778, #9123, #8190, #10684, #2293, #10739, #4057, #8288, #671, #3124, #7350, #4885, #1510, #6579, #3074, #7299, #6521, #8244, #8135, #576, #1359, #7402, #2340, #523, #9172, #10623, #2191, #7458, #10784, #628, #4940, #6472, #3909, #3220, #8968, #10837, #8343, #6629, #4008, #10008, #3960, #9853, #9798, #2240, #1460, #2388, #4726, #5620, #9015, #3174, #9958, #1407, #5729, #728, #1559, #4785, #9903, #5676, #9071, #7241, #3021, #6415, #936, #779, #2499, #1615, #10262, #882, #8497, #4110, #4158, #7508, #4208, #5044, #5149, #1835, #6834, #4315, #10890, #7725, #6890, #9280, #1672, #2670, #10102, #6049, #3380, #5206, #8609, #10936, #6676, #2440, #1719, #9436, #5993, #8444, #7559, #10157, #7613, #103, #8553, #3488, #714, #829, #3327, #9381, #10205, #6783, #4261, #7669, #1776, #5940, #5832, #3281, #9230, #2605, #52, #2553, #6728, #10052, #9326, #4991, #8395, #5887, #5094, #3436, #1944, #1044, #7834, #10496, #3779, #8837, #5377, #6163, #2952, #10555, #2895 ),
 ( #331, #4543, #4604, #1887, #7002, #161, #5493, #2059, #6226, #3547, #5258, #5315, #988, #10380, #10321, #4433, #8008, #8726, #8662, #5431, #273, #218, #1108, #393, #6338, #6283, #6945, #4367, #8783, #7949, #9608, #9668, #7779, #2724, #6107, #7894, #3718, #1224, #4490, #3658, #2002, #7117, #9492, #9722, #7172, #3604, #2116, #2776, #9551, #7054, #10435, #2839, #1164, #3061, #564, #9784, #661, #7445, #2173, #1498, #7391, #10770, #1444, #3008, #5553, #9946, #4042, #1392, #452, #5606, #617, #4713, #3893, #9840, #9108, #4874, #9001, #3160, #10826, #1344, #4821, #6564, #3210, #8121, #2278, #3996, #2329, #6397, #9995, #4770, #8231, #7286, #5711, #3110, #8277, #6617, #2378, #9888, #8898, #8175, #1284, #6507, #4661, #8069, #5660, #3836, #3943, #7337, #8954, #509, #7227, #10607, #2227, #10667, #6458, #10726, #9059, #2755, #2489, #10091, #10980, #9471, #9161, #7872, #193, #717, #8704, #4927, #1865, #3577, #6140, #6666, #5033, #10926, #8432, #10042, #1079, #4467, #2427, #9526, #4404, #7814, #5236, #10879, #5818, #6979, #252, #9266, #8325, #5873, #8640, #1601, #766, #6714, #1919, #5292, #1659, #10357, #3635, #9217, #1020, #7033, #10411, #4981, #10142, #5767, #1545, #3268, #4098, #817, #7495, #4148, #8382, #3369, #7546, #3315, #4196, #6770, #7600, #2698, #6082, #8043, #9586, #3871, #3817, #9815, #10532, #1261, #7927, #6261, #1978, #8931, #3754, #2037, #4695, #5527, #10472, #10643, #7207, #7093, #3925, #307, #2155, #2932, #5348, #1323, #8874, #5411, #8103, #6371, #6434, #3691, #8815, #8761, #7315, #7262, #432, #1142, #2872, #7152, #2812, #1198, #4524, #9647, #2209, #6317, #4578, #3042, #2093, #7984, #9701, #5589, #8156, #485, #371, #6198, #10587, #9759, #2985, #8984, #5467, #4641, #1375, #4747, #545, #7529, #645, #10910, #3299, #7421, #1579, #2465, #3143, #3245, #4963, #9249, #6541, #4078, #5798, #9195, #8206, #799, #10805, #6650, #5695, #8364, #4905, #749, #5854, #10025, #695, #2408, #9978, #6695, #8305, #6490, #4133, #7479, #10070, #3195, #9142, #4805, #9925, #9871, #1636, #4025, #2313, #5014, #8416, #7370, #4177, #10858, #3981, #10704, #597, #3093, #6597, #2259, #5640, #5748, #9090, #9035, #1426, #10754, #1479, #4856, #8262, #2360, #1530, #1796, #10121, #848, #8519, #1067, #2573, #5910, #19, #184, #899, #8463, #8629, #6854, #7634, #4280, #3564, #1906, #9456, #2520, #7577, #954, #3509, #5167, #5223, #10958, #9300, #1690, #3455, #6913, #4389, #7690, #72, #8576, #123, #3347, #9512, #1854, #5065, #10345, #6749, #10282, #1007, #7801, #4229, #10224, #1740, #2626, #3397, #2742, #6126, #6805, #6964, #6071, #5277, #2687, #10177, #5959, #8686, #9347, #6015, #5114, #9402, #4333, #7745, #10457, #8027, #9572, #8747, #5515, #7245, #7971, #7019, #1185, #7192, #293, #2859 ) ),
 .UNSPECIFIED., .F., .F., .F. ) 
 B_SPLINE_SURFACE_WITH_KNOTS ( ( 2, 2 ),
 ( 3, 2, 2, 2, 2, 2, 2, 2, 2, 2, 2, 2, 2, 2, 2, 2, 2, 2, 2, 2, 2, 2, 2, 2, 2, 2, 2, 2, 2, 2, 2, 2, 2, 2, 2, 2, 2, 2, 2, 2, 2, 2, 2, 2, 2, 2, 2, 2, 2, 2, 2, 2, 2, 2, 2, 2, 2, 2, 2, 2, 2, 2, 2, 2, 2, 2, 2, 2, 2, 2, 2, 2, 2, 2, 2, 2, 2, 2, 2, 2, 2, 2, 2, 2, 2, 2, 2, 2, 2, 2, 2, 2, 2, 2, 2, 2, 2, 2, 2, 2, 2, 2, 2, 2, 2, 2, 2, 2, 2, 2, 2, 2, 2, 2, 2, 2, 2, 2, 2, 2, 2, 2, 2, 2, 2, 2, 2, 2, 2, 2, 2, 2, 2, 2, 2, 2, 2, 2, 2, 2, 2, 2, 2, 2, 2, 2, 2, 2, 2, 2, 2, 2, 2, 2, 2, 2, 2, 2, 2, 2, 2, 2, 2, 2, 2, 2, 2, 2, 2, 2, 2, 2, 2, 2, 2, 2, 2, 2, 2, 2, 2, 2, 2, 2, 2, 2, 2, 2, 2, 2, 2, 2, 3 ),
 ( 0.000000000000000000, 1.000000000000000000 ),
 ( 0.000000000000000000, 0.005208333333333333044, 0.01041666666666666609, 0.01562500000000000000, 0.02083333333333333218, 0.02604166666666666782, 0.03125000000000000000, 0.03645833333333333565, 0.04166666666666666435, 0.04687500000000000000, 0.05208333333333333565, 0.05729166666666666435, 0.06250000000000000000, 0.06770833333333332871, 0.07291666666666667129, 0.07812500000000000000, 0.08333333333333332871, 0.08854166666666667129, 0.09375000000000000000, 0.09895833333333332871, 0.1041666666666666713, 0.1093750000000000000, 0.1145833333333333287, 0.1197916666666666713, 0.1250000000000000000, 0.1302083333333333426, 0.1354166666666666574, 0.1406250000000000000, 0.1458333333333333426, 0.1510416666666666574, 0.1562500000000000000, 0.1614583333333333426, 0.1666666666666666574, 0.1718750000000000000, 0.1770833333333333426, 0.1822916666666666574, 0.1875000000000000000, 0.1927083333333333426, 0.1979166666666666574, 0.2031250000000000000, 0.2083333333333333426, 0.2135416666666666574, 0.2187500000000000000, 0.2239583333333333426, 0.2291666666666666574, 0.2343750000000000000, 0.2395833333333333426, 0.2447916666666666574, 0.2500000000000000000, 0.2552083333333333148, 0.2604166666666666852, 0.2656250000000000000, 0.2708333333333333148, 0.2760416666666666852, 0.2812500000000000000, 0.2864583333333333148, 0.2916666666666666852, 0.2968750000000000000, 0.3020833333333333148, 0.3072916666666666852, 0.3125000000000000000, 0.3177083333333333148, 0.3229166666666666852, 0.3281250000000000000, 0.3333333333333333148, 0.3385416666666666852, 0.3437500000000000000, 0.3489583333333333148, 0.3541666666666666852, 0.3593750000000000000, 0.3645833333333333148, 0.3697916666666666852, 0.3750000000000000000, 0.3802083333333333148, 0.3854166666666666852, 0.3906250000000000000, 0.3958333333333333148, 0.4010416666666666852, 0.4062500000000000000, 0.4114583333333333148, 0.4166666666666666852, 0.4218750000000000000, 0.4270833333333333148, 0.4322916666666666852, 0.4375000000000000000, 0.4427083333333333148, 0.4479166666666666852, 0.4531250000000000000, 0.4583333333333333148, 0.4635416666666666852, 0.4687500000000000000, 0.4739583333333333148, 0.4791666666666666852, 0.4843750000000000000, 0.4895833333333333148, 0.4947916666666666852, 0.5000000000000000000, 0.5052083333333333703, 0.5104166666666666297, 0.5156250000000000000, 0.5208333333333333703, 0.5260416666666666297, 0.5312500000000000000, 0.5364583333333333703, 0.5416666666666666297, 0.5468750000000000000, 0.5520833333333333703, 0.5572916666666666297, 0.5625000000000000000, 0.5677083333333333703, 0.5729166666666666297, 0.5781250000000000000, 0.5833333333333333703, 0.5885416666666666297, 0.5937500000000000000, 0.5989583333333333703, 0.6041666666666666297, 0.6093750000000000000, 0.6145833333333333703, 0.6197916666666666297, 0.6250000000000000000, 0.6302083333333333703, 0.6354166666666666297, 0.6406250000000000000, 0.6458333333333333703, 0.6510416666666666297, 0.6562500000000000000, 0.6614583333333333703, 0.6666666666666666297, 0.6718750000000000000, 0.6770833333333333703, 0.6822916666666666297, 0.6875000000000000000, 0.6927083333333333703, 0.6979166666666666297, 0.7031250000000000000, 0.7083333333333333703, 0.7135416666666666297, 0.7187500000000000000, 0.7239583333333333703, 0.7291666666666666297, 0.7343750000000000000, 0.7395833333333333703, 0.7447916666666666297, 0.7500000000000000000, 0.7552083333333333703, 0.7604166666666666297, 0.7656250000000000000, 0.7708333333333333703, 0.7760416666666666297, 0.7812500000000000000, 0.7864583333333333703, 0.7916666666666666297, 0.7968750000000000000, 0.8020833333333333703, 0.8072916666666666297, 0.8125000000000000000, 0.8177083333333333703, 0.8229166666666666297, 0.8281250000000000000, 0.8333333333333333703, 0.8385416666666666297, 0.8437500000000000000, 0.8489583333333333703, 0.8541666666666666297, 0.8593750000000000000, 0.8645833333333333703, 0.8697916666666666297, 0.8750000000000000000, 0.8802083333333333703, 0.8854166666666666297, 0.8906250000000000000, 0.8958333333333333703, 0.9010416666666666297, 0.9062500000000000000, 0.9114583333333333703, 0.9166666666666666297, 0.9218750000000000000, 0.9270833333333333703, 0.9322916666666666297, 0.9375000000000000000, 0.9427083333333333703, 0.9479166666666666297, 0.9531250000000000000, 0.9583333333333333703, 0.9635416666666666297, 0.9687500000000000000, 0.9739583333333333703, 0.9791666666666666297, 0.9843750000000000000, 0.9895833333333333703, 0.9947916666666666297, 1.000000000000000000 ),
 .UNSPECIFIED. ) 
 GEOMETRIC_REPRESENTATION_ITEM ( )  RATIONAL_B_SPLINE_SURFACE ( (
 ( 1.000000000000000000, 0.8660254037844387076, 1.000000000000000000, 0.8660254037844387076, 1.000000000000000000, 0.8660254037844387076, 1.000000000000000000, 0.8660254037844387076, 1.000000000000000000, 0.8660254037844387076, 1.000000000000000000, 0.8660254037844387076, 1.000000000000000000, 0.8660254037844387076, 1.000000000000000000, 0.8660254037844387076, 1.000000000000000000, 0.8660254037844387076, 1.000000000000000000, 0.8660254037844387076, 1.000000000000000000, 0.8660254037844387076, 1.000000000000000000, 0.8660254037844387076, 1.000000000000000000, 0.8660254037844387076, 1.000000000000000000, 0.8660254037844387076, 1.000000000000000000, 0.8660254037844387076, 1.000000000000000000, 0.8660254037844387076, 1.000000000000000000, 0.8660254037844387076, 1.000000000000000000, 0.8660254037844387076, 1.000000000000000000, 0.8660254037844387076, 1.000000000000000000, 0.8660254037844387076, 1.000000000000000000, 0.8660254037844387076, 1.000000000000000000, 0.8660254037844387076, 1.000000000000000000, 0.8660254037844387076, 1.000000000000000000, 0.8660254037844387076, 1.000000000000000000, 0.8660254037844387076, 1.000000000000000000, 0.8660254037844387076, 1.000000000000000000, 0.8660254037844387076, 1.000000000000000000, 0.8660254037844387076, 1.000000000000000000, 0.8660254037844387076, 1.000000000000000000, 0.8660254037844387076, 1.000000000000000000, 0.8660254037844387076, 1.000000000000000000, 0.8660254037844387076, 1.000000000000000000, 0.8660254037844387076, 1.000000000000000000, 0.8660254037844387076, 1.000000000000000000, 0.8660254037844387076, 1.000000000000000000, 0.8660254037844387076, 1.000000000000000000, 0.8660254037844387076, 1.000000000000000000, 0.8660254037844387076, 1.000000000000000000, 0.8660254037844387076, 1.000000000000000000, 0.8660254037844387076, 1.000000000000000000, 0.8660254037844387076, 1.000000000000000000, 0.8660254037844387076, 1.000000000000000000, 0.8660254037844387076, 1.000000000000000000, 0.8660254037844387076, 1.000000000000000000, 0.8660254037844387076, 1.000000000000000000, 0.8660254037844387076, 1.000000000000000000, 0.8660254037844387076, 1.000000000000000000, 0.8660254037844387076, 1.000000000000000000, 0.8660254037844387076, 1.000000000000000000, 0.8660254037844387076, 1.000000000000000000, 0.8660254037844387076, 1.000000000000000000, 0.8660254037844387076, 1.000000000000000000, 0.8660254037844387076, 1.000000000000000000, 0.8660254037844387076, 1.000000000000000000, 0.8660254037844387076, 1.000000000000000000, 0.8660254037844387076, 1.000000000000000000, 0.8660254037844387076, 1.000000000000000000, 0.8660254037844387076, 1.000000000000000000, 0.8660254037844387076, 1.000000000000000000, 0.8660254037844387076, 1.000000000000000000, 0.8660254037844387076, 1.000000000000000000, 0.8660254037844387076, 1.000000000000000000, 0.8660254037844387076, 1.000000000000000000, 0.8660254037844387076, 1.000000000000000000, 0.8660254037844387076, 1.000000000000000000, 0.8660254037844387076, 1.000000000000000000, 0.8660254037844387076, 1.000000000000000000, 0.8660254037844387076, 1.000000000000000000, 0.8660254037844387076, 1.000000000000000000, 0.8660254037844387076, 1.000000000000000000, 0.8660254037844387076, 1.000000000000000000, 0.8660254037844387076, 1.000000000000000000, 0.8660254037844387076, 1.000000000000000000, 0.8660254037844387076, 1.000000000000000000, 0.8660254037844387076, 1.000000000000000000, 0.8660254037844387076, 1.000000000000000000, 0.8660254037844387076, 1.000000000000000000, 0.8660254037844387076, 1.000000000000000000, 0.8660254037844387076, 1.000000000000000000, 0.8660254037844387076, 1.000000000000000000, 0.8660254037844387076, 1.000000000000000000, 0.8660254037844387076, 1.000000000000000000, 0.8660254037844387076, 1.000000000000000000, 0.8660254037844387076, 1.000000000000000000, 0.8660254037844387076, 1.000000000000000000, 0.8660254037844387076, 1.000000000000000000, 0.8660254037844387076, 1.000000000000000000, 0.8660254037844387076, 1.000000000000000000, 0.8660254037844387076, 1.000000000000000000, 0.8660254037844387076, 1.000000000000000000, 0.8660254037844387076, 1.000000000000000000, 0.8660254037844387076, 1.000000000000000000, 0.8660254037844387076, 1.000000000000000000, 0.8660254037844387076, 1.000000000000000000, 0.8660254037844387076, 1.000000000000000000, 0.8660254037844387076, 1.000000000000000000, 0.8660254037844387076, 1.000000000000000000, 0.8660254037844387076, 1.000000000000000000, 0.8660254037844387076, 1.000000000000000000, 0.8660254037844387076, 1.000000000000000000, 0.8660254037844387076, 1.000000000000000000, 0.8660254037844387076, 1.000000000000000000, 0.8660254037844387076, 1.000000000000000000, 0.8660254037844387076, 1.000000000000000000, 0.8660254037844387076, 1.000000000000000000, 0.8660254037844387076, 1.000000000000000000, 0.8660254037844387076, 1.000000000000000000, 0.8660254037844387076, 1.000000000000000000, 0.8660254037844387076, 1.000000000000000000, 0.8660254037844387076, 1.000000000000000000, 0.8660254037844387076, 1.000000000000000000, 0.8660254037844387076, 1.000000000000000000, 0.8660254037844387076, 1.000000000000000000, 0.8660254037844387076, 1.000000000000000000, 0.8660254037844387076, 1.000000000000000000, 0.8660254037844387076, 1.000000000000000000, 0.8660254037844387076, 1.000000000000000000, 0.8660254037844387076, 1.000000000000000000, 0.8660254037844387076, 1.000000000000000000, 0.8660254037844387076, 1.000000000000000000, 0.8660254037844387076, 1.000000000000000000, 0.8660254037844387076, 1.000000000000000000, 0.8660254037844387076, 1.000000000000000000, 0.8660254037844387076, 1.000000000000000000, 0.8660254037844387076, 1.000000000000000000, 0.8660254037844387076, 1.000000000000000000, 0.8660254037844387076, 1.000000000000000000, 0.8660254037844387076, 1.000000000000000000, 0.8660254037844387076, 1.000000000000000000, 0.8660254037844387076, 1.000000000000000000, 0.8660254037844387076, 1.000000000000000000, 0.8660254037844387076, 1.000000000000000000, 0.8660254037844387076, 1.000000000000000000, 0.8660254037844387076, 1.000000000000000000, 0.8660254037844387076, 1.000000000000000000, 0.8660254037844387076, 1.000000000000000000, 0.8660254037844387076, 1.000000000000000000, 0.8660254037844387076, 1.000000000000000000, 0.8660254037844387076, 1.000000000000000000, 0.8660254037844387076, 1.000000000000000000, 0.8660254037844387076, 1.000000000000000000, 0.8660254037844387076, 1.000000000000000000, 0.8660254037844387076, 1.000000000000000000, 0.8660254037844387076, 1.000000000000000000, 0.8660254037844387076, 1.000000000000000000, 0.8660254037844387076, 1.000000000000000000, 0.8660254037844387076, 1.000000000000000000, 0.8660254037844387076, 1.000000000000000000, 0.8660254037844387076, 1.000000000000000000, 0.8660254037844387076, 1.000000000000000000, 0.8660254037844387076, 1.000000000000000000, 0.8660254037844387076, 1.000000000000000000, 0.8660254037844387076, 1.000000000000000000, 0.8660254037844387076, 1.000000000000000000, 0.8660254037844387076, 1.000000000000000000, 0.8660254037844387076, 1.000000000000000000, 0.8660254037844387076, 1.000000000000000000, 0.8660254037844387076, 1.000000000000000000, 0.8660254037844387076, 1.000000000000000000, 0.8660254037844387076, 1.000000000000000000, 0.8660254037844387076, 1.000000000000000000, 0.8660254037844387076, 1.000000000000000000, 0.8660254037844387076, 1.000000000000000000, 0.8660254037844387076, 1.000000000000000000, 0.8660254037844387076, 1.000000000000000000, 0.8660254037844387076, 1.000000000000000000, 0.8660254037844387076, 1.000000000000000000, 0.8660254037844387076, 1.000000000000000000, 0.8660254037844387076, 1.000000000000000000, 0.8660254037844387076, 1.000000000000000000, 0.8660254037844387076, 1.000000000000000000, 0.8660254037844387076, 1.000000000000000000, 0.8660254037844387076, 1.000000000000000000, 0.8660254037844387076, 1.000000000000000000, 0.8660254037844387076, 1.000000000000000000, 0.8660254037844387076, 1.000000000000000000, 0.8660254037844387076, 1.000000000000000000, 0.8660254037844387076, 1.000000000000000000, 0.8660254037844387076, 1.000000000000000000, 0.8660254037844387076, 1.000000000000000000, 0.8660254037844387076, 1.000000000000000000, 0.8660254037844387076, 1.000000000000000000, 0.8660254037844387076, 1.000000000000000000, 0.8660254037844387076, 1.000000000000000000, 0.8660254037844387076, 1.000000000000000000, 0.8660254037844387076, 1.000000000000000000, 0.8660254037844387076, 1.000000000000000000, 0.8660254037844387076, 1.000000000000000000, 0.8660254037844387076, 1.000000000000000000, 0.8660254037844387076, 1.000000000000000000, 0.8660254037844387076, 1.000000000000000000, 0.8660254037844387076, 1.000000000000000000),
 ( 1.000000000000000000, 0.8660254037844387076, 1.000000000000000000, 0.8660254037844387076, 1.000000000000000000, 0.8660254037844387076, 1.000000000000000000, 0.8660254037844387076, 1.000000000000000000, 0.8660254037844387076, 1.000000000000000000, 0.8660254037844387076, 1.000000000000000000, 0.8660254037844387076, 1.000000000000000000, 0.8660254037844387076, 1.000000000000000000, 0.8660254037844387076, 1.000000000000000000, 0.8660254037844387076, 1.000000000000000000, 0.8660254037844387076, 1.000000000000000000, 0.8660254037844387076, 1.000000000000000000, 0.8660254037844387076, 1.000000000000000000, 0.8660254037844387076, 1.000000000000000000, 0.8660254037844387076, 1.000000000000000000, 0.8660254037844387076, 1.000000000000000000, 0.8660254037844387076, 1.000000000000000000, 0.8660254037844387076, 1.000000000000000000, 0.8660254037844387076, 1.000000000000000000, 0.8660254037844387076, 1.000000000000000000, 0.8660254037844387076, 1.000000000000000000, 0.8660254037844387076, 1.000000000000000000, 0.8660254037844387076, 1.000000000000000000, 0.8660254037844387076, 1.000000000000000000, 0.8660254037844387076, 1.000000000000000000, 0.8660254037844387076, 1.000000000000000000, 0.8660254037844387076, 1.000000000000000000, 0.8660254037844387076, 1.000000000000000000, 0.8660254037844387076, 1.000000000000000000, 0.8660254037844387076, 1.000000000000000000, 0.8660254037844387076, 1.000000000000000000, 0.8660254037844387076, 1.000000000000000000, 0.8660254037844387076, 1.000000000000000000, 0.8660254037844387076, 1.000000000000000000, 0.8660254037844387076, 1.000000000000000000, 0.8660254037844387076, 1.000000000000000000, 0.8660254037844387076, 1.000000000000000000, 0.8660254037844387076, 1.000000000000000000, 0.8660254037844387076, 1.000000000000000000, 0.8660254037844387076, 1.000000000000000000, 0.8660254037844387076, 1.000000000000000000, 0.8660254037844387076, 1.000000000000000000, 0.8660254037844387076, 1.000000000000000000, 0.8660254037844387076, 1.000000000000000000, 0.8660254037844387076, 1.000000000000000000, 0.8660254037844387076, 1.000000000000000000, 0.8660254037844387076, 1.000000000000000000, 0.8660254037844387076, 1.000000000000000000, 0.8660254037844387076, 1.000000000000000000, 0.8660254037844387076, 1.000000000000000000, 0.8660254037844387076, 1.000000000000000000, 0.8660254037844387076, 1.000000000000000000, 0.8660254037844387076, 1.000000000000000000, 0.8660254037844387076, 1.000000000000000000, 0.8660254037844387076, 1.000000000000000000, 0.8660254037844387076, 1.000000000000000000, 0.8660254037844387076, 1.000000000000000000, 0.8660254037844387076, 1.000000000000000000, 0.8660254037844387076, 1.000000000000000000, 0.8660254037844387076, 1.000000000000000000, 0.8660254037844387076, 1.000000000000000000, 0.8660254037844387076, 1.000000000000000000, 0.8660254037844387076, 1.000000000000000000, 0.8660254037844387076, 1.000000000000000000, 0.8660254037844387076, 1.000000000000000000, 0.8660254037844387076, 1.000000000000000000, 0.8660254037844387076, 1.000000000000000000, 0.8660254037844387076, 1.000000000000000000, 0.8660254037844387076, 1.000000000000000000, 0.8660254037844387076, 1.000000000000000000, 0.8660254037844387076, 1.000000000000000000, 0.8660254037844387076, 1.000000000000000000, 0.8660254037844387076, 1.000000000000000000, 0.8660254037844387076, 1.000000000000000000, 0.8660254037844387076, 1.000000000000000000, 0.8660254037844387076, 1.000000000000000000, 0.8660254037844387076, 1.000000000000000000, 0.8660254037844387076, 1.000000000000000000, 0.8660254037844387076, 1.000000000000000000, 0.8660254037844387076, 1.000000000000000000, 0.8660254037844387076, 1.000000000000000000, 0.8660254037844387076, 1.000000000000000000, 0.8660254037844387076, 1.000000000000000000, 0.8660254037844387076, 1.000000000000000000, 0.8660254037844387076, 1.000000000000000000, 0.8660254037844387076, 1.000000000000000000, 0.8660254037844387076, 1.000000000000000000, 0.8660254037844387076, 1.000000000000000000, 0.8660254037844387076, 1.000000000000000000, 0.8660254037844387076, 1.000000000000000000, 0.8660254037844387076, 1.000000000000000000, 0.8660254037844387076, 1.000000000000000000, 0.8660254037844387076, 1.000000000000000000, 0.8660254037844387076, 1.000000000000000000, 0.8660254037844387076, 1.000000000000000000, 0.8660254037844387076, 1.000000000000000000, 0.8660254037844387076, 1.000000000000000000, 0.8660254037844387076, 1.000000000000000000, 0.8660254037844387076, 1.000000000000000000, 0.8660254037844387076, 1.000000000000000000, 0.8660254037844387076, 1.000000000000000000, 0.8660254037844387076, 1.000000000000000000, 0.8660254037844387076, 1.000000000000000000, 0.8660254037844387076, 1.000000000000000000, 0.8660254037844387076, 1.000000000000000000, 0.8660254037844387076, 1.000000000000000000, 0.8660254037844387076, 1.000000000000000000, 0.8660254037844387076, 1.000000000000000000, 0.8660254037844387076, 1.000000000000000000, 0.8660254037844387076, 1.000000000000000000, 0.8660254037844387076, 1.000000000000000000, 0.8660254037844387076, 1.000000000000000000, 0.8660254037844387076, 1.000000000000000000, 0.8660254037844387076, 1.000000000000000000, 0.8660254037844387076, 1.000000000000000000, 0.8660254037844387076, 1.000000000000000000, 0.8660254037844387076, 1.000000000000000000, 0.8660254037844387076, 1.000000000000000000, 0.8660254037844387076, 1.000000000000000000, 0.8660254037844387076, 1.000000000000000000, 0.8660254037844387076, 1.000000000000000000, 0.8660254037844387076, 1.000000000000000000, 0.8660254037844387076, 1.000000000000000000, 0.8660254037844387076, 1.000000000000000000, 0.8660254037844387076, 1.000000000000000000, 0.8660254037844387076, 1.000000000000000000, 0.8660254037844387076, 1.000000000000000000, 0.8660254037844387076, 1.000000000000000000, 0.8660254037844387076, 1.000000000000000000, 0.8660254037844387076, 1.000000000000000000, 0.8660254037844387076, 1.000000000000000000, 0.8660254037844387076, 1.000000000000000000, 0.8660254037844387076, 1.000000000000000000, 0.8660254037844387076, 1.000000000000000000, 0.8660254037844387076, 1.000000000000000000, 0.8660254037844387076, 1.000000000000000000, 0.8660254037844387076, 1.000000000000000000, 0.8660254037844387076, 1.000000000000000000, 0.8660254037844387076, 1.000000000000000000, 0.8660254037844387076, 1.000000000000000000, 0.8660254037844387076, 1.000000000000000000, 0.8660254037844387076, 1.000000000000000000, 0.8660254037844387076, 1.000000000000000000, 0.8660254037844387076, 1.000000000000000000, 0.8660254037844387076, 1.000000000000000000, 0.8660254037844387076, 1.000000000000000000, 0.8660254037844387076, 1.000000000000000000, 0.8660254037844387076, 1.000000000000000000, 0.8660254037844387076, 1.000000000000000000, 0.8660254037844387076, 1.000000000000000000, 0.8660254037844387076, 1.000000000000000000, 0.8660254037844387076, 1.000000000000000000, 0.8660254037844387076, 1.000000000000000000, 0.8660254037844387076, 1.000000000000000000, 0.8660254037844387076, 1.000000000000000000, 0.8660254037844387076, 1.000000000000000000, 0.8660254037844387076, 1.000000000000000000, 0.8660254037844387076, 1.000000000000000000, 0.8660254037844387076, 1.000000000000000000, 0.8660254037844387076, 1.000000000000000000, 0.8660254037844387076, 1.000000000000000000, 0.8660254037844387076, 1.000000000000000000, 0.8660254037844387076, 1.000000000000000000, 0.8660254037844387076, 1.000000000000000000, 0.8660254037844387076, 1.000000000000000000, 0.8660254037844387076, 1.000000000000000000, 0.8660254037844387076, 1.000000000000000000, 0.8660254037844387076, 1.000000000000000000, 0.8660254037844387076, 1.000000000000000000, 0.8660254037844387076, 1.000000000000000000, 0.8660254037844387076, 1.000000000000000000, 0.8660254037844387076, 1.000000000000000000, 0.8660254037844387076, 1.000000000000000000, 0.8660254037844387076, 1.000000000000000000, 0.8660254037844387076, 1.000000000000000000, 0.8660254037844387076, 1.000000000000000000, 0.8660254037844387076, 1.000000000000000000, 0.8660254037844387076, 1.000000000000000000, 0.8660254037844387076, 1.000000000000000000, 0.8660254037844387076, 1.000000000000000000, 0.8660254037844387076, 1.000000000000000000, 0.8660254037844387076, 1.000000000000000000, 0.8660254037844387076, 1.000000000000000000, 0.8660254037844387076, 1.000000000000000000, 0.8660254037844387076, 1.000000000000000000, 0.8660254037844387076, 1.000000000000000000, 0.8660254037844387076, 1.000000000000000000, 0.8660254037844387076, 1.000000000000000000, 0.8660254037844387076, 1.000000000000000000, 0.8660254037844387076, 1.000000000000000000, 0.8660254037844387076, 1.000000000000000000, 0.8660254037844387076, 1.000000000000000000) ) ) 
 REPRESENTATION_ITEM ( '' )  SURFACE ( )  );
#10830 = CARTESIAN_POINT ( 'NONE',  ( -62.49999999999998579, 15.88541666598386826, 2.366025403784441483 ) ) ;
#10831 = CARTESIAN_POINT ( 'NONE',  ( -61.13531646874998415, 11.39062499965860020, 1.500000000000002220 ) ) ;
#10832 = FACE_OUTER_BOUND ( 'NONE', #4488, .T. ) ;
#10833 = VERTEX_POINT ( 'NONE', #4322 ) ;
#10834 = DIRECTION ( 'NONE',  ( 0.000000000000000000, -0.000000000000000000, 1.000000000000000000 ) ) ;
#10835 = DIRECTION ( 'NONE',  ( -1.000000000000000000, -0.000000000000000000, -0.000000000000000000 ) ) ;
#10836 = EDGE_CURVE ( 'NONE', #4938, #9653, #2676, .T. ) ;
#10837 = CARTESIAN_POINT ( 'NONE',  ( -62.86468353124998742, 13.97395833299193413, 1.999225269531025972 ) ) ;
#10838 = CARTESIAN_POINT ( 'NONE',  ( -61.99999999999998579, 16.00000000000000000, 1.500000000000002220 ) ) ;
#10839 = CARTESIAN_POINT ( 'NONE',  ( -61.49999999999998579, 14.45833333333333393, 2.366025403784441927 ) ) ;
#10840 = CYLINDRICAL_SURFACE ( 'NONE', #1015, 0.9999999999999981126 ) ;
#10841 = CARTESIAN_POINT ( 'NONE',  ( -61.56765823437498142, 12.68229166632526805, 0.7511620957034663704 ) ) ;
#10842 = CARTESIAN_POINT ( 'NONE',  ( -61.13531646874998415, 15.41145833299193413, 1.000774730468978468 ) ) ;
#10843 = EDGE_CURVE ( 'NONE', #3152, #544, #4374, .T. ) ;
#10844 = DIRECTION ( 'NONE',  ( -1.224646799147355672E-16, 1.000000000000000000, 0.000000000000000000 ) ) ;
#10845 = CONTEXT_DEPENDENT_SHAPE_REPRESENTATION ( #1456, #9900 ) ;
#10846 = DIRECTION ( 'NONE',  ( 1.000000000000000000, 0.000000000000000000, -0.000000000000000000 ) ) ;
#10847 = CARTESIAN_POINT ( 'NONE',  ( -62.86468353124998742, 8.286458332991934128, 1.999225269531025972 ) ) ;
#10848 = CARTESIAN_POINT ( 'NONE',  ( -46.99999999999998579, -18.00000000000001066, 3.000000000000000000 ) ) ;
#10849 = ORIENTED_EDGE ( 'NONE', *, *, #4658, .T. ) ;
#10850 = DIRECTION ( 'NONE',  ( 0.000000000000000000, 0.000000000000000000, -1.000000000000000000 ) ) ;
#10851 = DIRECTION ( 'NONE',  ( 0.000000000000000000, 0.000000000000000000, 1.000000000000000000 ) ) ;
#10852 = CIRCLE ( 'NONE', #6059, 1.100000000000003642 ) ;
#10853 = CARTESIAN_POINT ( 'NONE',  ( -62.43234176562499016, 14.24479166632526983, 2.248837904296538071 ) ) ;
#10854 = CARTESIAN_POINT ( 'NONE',  ( -61.13531646874998415, 9.557291666325269830, 1.999225269531026417 ) ) ;
#10855 = CARTESIAN_POINT ( 'NONE',  ( -61.56765823437498852, 15.34895833299193590, 2.248837904296538515 ) ) ;
#10856 = DIRECTION ( 'NONE',  ( -0.000000000000000000, -1.000000000000000000, -0.000000000000000000 ) ) ;
#10857 = VERTEX_POINT ( 'NONE', #7008 ) ;
#10858 = CARTESIAN_POINT ( 'NONE',  ( -61.99999999999998579, 14.06250000000000178, 0.3452994616207497591 ) ) ;
#10859 = CARTESIAN_POINT ( 'NONE',  ( -62.86468353124998032, 9.244791666325268054, 1.000774730468978024 ) ) ;
#10860 = CARTESIAN_POINT ( 'NONE',  ( -61.99999999999998579, 12.53124999931720396, 0.3452994616207497591 ) ) ;
#10861 = VECTOR ( 'NONE', #3375, 1000.000000000000000 ) ;
#10862 = EDGE_CURVE ( 'NONE', #6385, #10637, #5384, .T. ) ;
#10863 = CARTESIAN_POINT ( 'NONE',  ( 140.0000000000000284, -8.000000000000000000, 3.000000000000000000 ) ) ;
#10864 = CARTESIAN_POINT ( 'NONE',  ( -62.43234176562498305, 13.91145833299193413, 0.7511620957034662593 ) ) ;
#10865 = CARTESIAN_POINT ( 'NONE',  ( -61.73205080756886076, 11.44866454968463110, 2.500000000000000000 ) ) ;
#10866 = EDGE_LOOP ( 'NONE', ( #2092, #527, #8938, #6550 ) ) ;
#10867 = CIRCLE ( 'NONE', #1482, 30.00000000000000000 ) ;
#10868 = AXIS2_PLACEMENT_3D ( 'NONE', #522, #7349, #5675 ) ;
#10869 = CARTESIAN_POINT ( 'NONE',  ( -62.43234176562498305, 12.22395833299193413, 0.7511620957034662593 ) ) ;
#10870 = DIRECTION ( 'NONE',  ( 1.000000000000000000, 0.000000000000000000, 0.000000000000000000 ) ) ;
#10871 = CYLINDRICAL_SURFACE ( 'NONE', #1036, 0.9999999999999981126 ) ;
#10872 = APPLICATION_CONTEXT ( 'automotive_design' ) ;
#10873 = EDGE_LOOP ( 'NONE', ( #4403, #10369, #4704, #3529 ) ) ;
#10874 = VECTOR ( 'NONE', #2747, 1000.000000000000000 ) ;
#10875 = CARTESIAN_POINT ( 'NONE',  ( -49.99999999999998579, -10.00000000000000888, 3.000000000000000000 ) ) ;
#10876 = VERTEX_POINT ( 'NONE', #7901 ) ;
#10877 = PLANE ( 'NONE',  #1623 ) ;
#10878 = EDGE_CURVE ( 'NONE', #6336, #10433, #7123, .T. ) ;
#10879 = CARTESIAN_POINT ( 'NONE',  ( -60.99999999999998579, 10.97916666666666607, 2.077350269189628840 ) ) ;
#10880 = CYLINDRICAL_SURFACE ( 'NONE', #1032, 0.9999999999999981126 ) ;
#10881 = PLANE ( 'NONE',  #9548 ) ;
#10882 = VECTOR ( 'NONE', #7338, 1000.000000000000000 ) ;
#10883 = CARTESIAN_POINT ( 'NONE',  ( -62.99999999999998579, 8.843749999317203958, 1.500000000000001998 ) ) ;
#10884 = CARTESIAN_POINT ( 'NONE',  ( -62.43234176562498305, 13.72395833299193413, 0.7511620957034662593 ) ) ;
#10885 = CARTESIAN_POINT ( 'NONE',  ( -61.99999999999997868, 10.68749999999999822, 2.500000000000002665 ) ) ;
#10886 = ORIENTED_EDGE ( 'NONE', *, *, #8401, .T. ) ;
#10887 = DIRECTION ( 'NONE',  ( 0.000000000000000000, -5.282956808509868713E-16, -1.000000000000000000 ) ) ;
#10888 = EDGE_LOOP ( 'NONE', ( #7651, #7767, #7663, #5623 ) ) ;
#10889 = CARTESIAN_POINT ( 'NONE',  ( -37.99999999999999289, -14.00000000000000888, 5.000000000000000000 ) ) ;
#10890 = CARTESIAN_POINT ( 'NONE',  ( -61.56765823437498142, 14.86979166632526805, 0.7511620957034663704 ) ) ;
#10891 = FACE_OUTER_BOUND ( 'NONE', #3535, .T. ) ;
#10892 = CARTESIAN_POINT ( 'NONE',  ( -61.99999999999998579, 9.906249999317202182, 2.500000000000002665 ) ) ;
#10893 =( BOUNDED_CURVE ( )  B_SPLINE_CURVE ( 2, ( #6786, #4264, #7672, #55, #10208, #6166, #10438, #2119, #455 ),
 .UNSPECIFIED., .F., .F. ) 
 B_SPLINE_CURVE_WITH_KNOTS ( ( 3, 2, 2, 2, 3 ),
 ( 0.1015625000000000833, 0.1041666666666666713, 0.1093750000000000000, 0.1145833333333333287, 0.1171875000000000278 ),
 .UNSPECIFIED. ) 
 CURVE ( )  GEOMETRIC_REPRESENTATION_ITEM ( )  RATIONAL_B_SPLINE_CURVE ( ( 0.9330127018922194093, 0.9330127018922215187, 1.000000000000000000, 0.8660254037844387076, 1.000000000000000000, 0.8660254037844387076, 1.000000000000000000, 0.9330127018922186322, 0.9330127018922194093 ) ) 
 REPRESENTATION_ITEM ( '' )  );
#10894 = FACE_OUTER_BOUND ( 'NONE', #5068, .T. ) ;
#10895 = CARTESIAN_POINT ( 'NONE',  ( -61.13531646874997705, 12.16145833299193413, 1.000774730468978468 ) ) ;
#10896 = CARTESIAN_POINT ( 'NONE',  ( -61.13531646874998415, 16.14062499965860198, 1.500000000000002220 ) ) ;
#10897 = CARTESIAN_POINT ( 'NONE',  ( 140.0000000000000284, -2.500000000000000000, 3.000000000000000000 ) ) ;
#10898 = DIRECTION ( 'NONE',  ( 0.000000000000000000, -1.000000000000000000, 0.000000000000000000 ) ) ;
#10899 = CARTESIAN_POINT ( 'NONE',  ( -61.13531646874998415, 8.161458332991935904, 1.000774730468978468 ) ) ;
#10900 = CARTESIAN_POINT ( 'NONE',  ( 1.084202172485504434E-16, 0.000000000000000000, 0.000000000000000000 ) ) ;
#10901 = ORIENTED_EDGE ( 'NONE', *, *, #3545, .T. ) ;
#10902 = DIRECTION ( 'NONE',  ( -0.000000000000000000, -1.000000000000000000, -0.000000000000000000 ) ) ;
#10903 = CARTESIAN_POINT ( 'NONE',  ( -62.26794919243111082, 12.57366454968463110, 0.5000000000000013323 ) ) ;
#10904 = EDGE_CURVE ( 'NONE', #1104, #4762, #7716, .T. ) ;
#10905 = CARTESIAN_POINT ( 'NONE',  ( -62.86468353124998032, 14.68229166632526805, 1.000774730468978024 ) ) ;
#10906 = CARTESIAN_POINT ( 'NONE',  ( -61.99999999999998579, 10.01562499965860020, 2.498450539062049724 ) ) ;
#10907 = CARTESIAN_POINT ( 'NONE',  ( -61.13531646874997705, 15.41145833299193590, 1.000774730468978468 ) ) ;
#10908 = DIRECTION ( 'NONE',  ( 0.000000000000000000, 0.000000000000000000, -1.000000000000000000 ) ) ;
#10909 = ORIENTED_EDGE ( 'NONE', *, *, #1987, .F. ) ;
#10910 = CARTESIAN_POINT ( 'NONE',  ( -62.99999999999998579, 13.14583333333333215, 2.077350269189627952 ) ) ;
#10911 = CARTESIAN_POINT ( 'NONE',  ( -61.13531646874997705, 8.411458332991934128, 1.000774730468978468 ) ) ;
#10912 = CARTESIAN_POINT ( 'NONE',  ( -62.49999999999998579, 11.30208333265053611, 0.6339745962155627357 ) ) ;
#10913 = CYLINDRICAL_SURFACE ( 'NONE', #1292, 0.9999999999999981126 ) ;
#10914 = CARTESIAN_POINT ( 'NONE',  ( -61.99999999999998579, 14.39062499965859843, 0.5015494609379544944 ) ) ;
#10915 = CARTESIAN_POINT ( 'NONE',  ( -61.99999999999998579, 11.56250000000000000, 0.5000000000000013323 ) ) ;
#10916 = ORIENTED_EDGE ( 'NONE', *, *, #479, .T. ) ;
#10917 = EDGE_CURVE ( 'NONE', #7283, #10003, #9674, .T. ) ;
#10918 = CARTESIAN_POINT ( 'NONE',  ( -61.56765823437498852, 13.34895833299193413, 2.248837904296538515 ) ) ;
#10919 = DIRECTION ( 'NONE',  ( -0.000000000000000000, -1.000000000000000000, -0.000000000000000000 ) ) ;
#10920 = ADVANCED_BREP_SHAPE_REPRESENTATION ( '', ( #1096, #2307 ), #4612 ) ;
#10921 = PRODUCT_DEFINITION_CONTEXT ( 'detailed design', #10293, 'design' ) ;
#10922 = CARTESIAN_POINT ( 'NONE',  ( 0.5477065543514035850, 2.408992218395923449E-16, 1.934182851860891672 ) ) ;
#10923 = ORIENTED_EDGE ( 'NONE', *, *, #10692, .T. ) ;
#10924 = CARTESIAN_POINT ( 'NONE',  ( -77.99999999999998579, 0.000000000000000000, 13.00000000000000178 ) ) ;
#10925 = EDGE_LOOP ( 'NONE', ( #6117, #7206 ) ) ;
#10926 = CARTESIAN_POINT ( 'NONE',  ( -60.99999999999998579, 10.77083333333333215, 0.9226497308103762673 ) ) ;
#10927 = ORIENTED_EDGE ( 'NONE', *, *, #4449, .F. ) ;
#10928 = CARTESIAN_POINT ( 'NONE',  ( -62.86468353124998742, 8.286458332991934128, 1.999225269531025972 ) ) ;
#10929 = CARTESIAN_POINT ( 'NONE',  ( 140.0000000000000284, 8.000000000000000000, 6.000000000000000000 ) ) ;
#10930 = CARTESIAN_POINT ( 'NONE',  ( -61.13531646874998415, 12.91145833299193590, 1.000774730468978468 ) ) ;
#10931 = DIRECTION ( 'NONE',  ( -1.000000000000000000, 0.000000000000000000, 0.000000000000000000 ) ) ;
#10932 = ORIENTED_EDGE ( 'NONE', *, *, #6909, .F. ) ;
#10933 = DIRECTION ( 'NONE',  ( -1.000000000000000000, 0.000000000000000000, 0.000000000000000000 ) ) ;
#10934 = ORIENTED_EDGE ( 'NONE', *, *, #8679, .F. ) ;
#10935 = CARTESIAN_POINT ( 'NONE',  ( -61.49999999999998579, 12.70833333333333393, 2.366025403784441927 ) ) ;
#10936 = CARTESIAN_POINT ( 'NONE',  ( -61.13531646874998415, 15.09895833299193413, 1.000774730468978468 ) ) ;
#10937 = LINE ( 'NONE', #5095, #8940 ) ;
#10938 = SURFACE_STYLE_FILL_AREA ( #4943 ) ;
#10939 = CARTESIAN_POINT ( 'NONE',  ( -61.49999999999998579, 10.79166666666666607, 0.6339745962155628467 ) ) ;
#10940 = CARTESIAN_POINT ( 'NONE',  ( -61.13531646874998415, 12.64062499965860198, 1.500000000000002220 ) ) ;
#10941 = CARTESIAN_POINT ( 'NONE',  ( -61.56765823437498142, 14.93229166632526805, 0.7511620957034663704 ) ) ;
#10942 = DIRECTION ( 'NONE',  ( 0.000000000000000000, 0.000000000000000000, -1.000000000000000000 ) ) ;
#10943 = CARTESIAN_POINT ( 'NONE',  ( -61.99999999999998579, 13.53124999931720041, 0.5000000000000013323 ) ) ;
#10944 = CARTESIAN_POINT ( 'NONE',  ( -61.13531646874998415, 9.161458332991935904, 1.000774730468978468 ) ) ;
#10945 =( REPRESENTATION_RELATIONSHIP ('NONE','NONE', #560, #6156 ) REPRESENTATION_RELATIONSHIP_WITH_TRANSFORMATION ( #3132 )SHAPE_REPRESENTATION_RELATIONSHIP( ) );
#10946 = DIRECTION ( 'NONE',  ( -0.000000000000000000, -1.000000000000000000, -0.000000000000000000 ) ) ;
#10947 = ORIENTED_EDGE ( 'NONE', *, *, #8053, .T. ) ;
#10948 = CARTESIAN_POINT ( 'NONE',  ( 145.0000000000000284, 5.500000000000000000, 0.000000000000000000 ) ) ;
#10949 = EDGE_CURVE ( 'NONE', #8992, #5874, #9616, .T. ) ;
#10950 = CARTESIAN_POINT ( 'NONE',  ( 0.000000000000000000, 0.2499999999999998335, -1.312875263449799101 ) ) ;
#10951 =( BOUNDED_CURVE ( )  B_SPLINE_CURVE ( 2, ( #7296, #463, #1237, #8130, #9680, #9734, #4673, #6468, #519 ),
 .UNSPECIFIED., .F., .T. ) 
 B_SPLINE_CURVE_WITH_KNOTS ( ( 3, 2, 2, 2, 3 ),
 ( 0.1328125000000000000, 0.1354166666666666574, 0.1406250000000000000, 0.1458333333333333426, 0.1484374999999999722 ),
 .UNSPECIFIED. ) 
 CURVE ( )  GEOMETRIC_REPRESENTATION_ITEM ( )  RATIONAL_B_SPLINE_CURVE ( ( 0.9330127018922194093, 0.9330127018922194093, 1.000000000000000000, 0.8660254037844387076, 1.000000000000000000, 0.8660254037844387076, 1.000000000000000000, 0.9330127018922200755, 0.9330127018922194093 ) ) 
 REPRESENTATION_ITEM ( '' )  );
#10952 = CARTESIAN_POINT ( 'NONE',  ( -61.56765823437498142, 13.61979166632526805, 0.7511620957034663704 ) ) ;
#10953 = CARTESIAN_POINT ( 'NONE',  ( -62.86468353124998742, 11.72395833299193413, 1.999225269531025972 ) ) ;
#10954 = VECTOR ( 'NONE', #5836, 1000.000000000000000 ) ;
#10955 = CARTESIAN_POINT ( 'NONE',  ( -62.86468353124999453, 15.26562499965860020, 1.500000000000002220 ) ) ;
#10956 = CARTESIAN_POINT ( 'NONE',  ( -61.49999999999998579, 14.51041666598387003, 0.6339745962155628467 ) ) ;
#10957 = ORIENTED_EDGE ( 'NONE', *, *, #5192, .F. ) ;
#10958 = CARTESIAN_POINT ( 'NONE',  ( -61.99999999999998579, 14.93749999999999822, 2.654700538379254571 ) ) ;
#10959 = PRODUCT ( 'slotted pan head screw_iso_ISO 1580 - M2 x 10 - 10N', 'slotted pan head screw_iso_ISO 1580 - M2 x 10 - 10N', '', ( #3029 ) ) ;
#10960 = CARTESIAN_POINT ( 'NONE',  ( -62.86468353124999453, 8.536458332991934128, 1.999225269531025750 ) ) ;
#10961 = CARTESIAN_POINT ( 'NONE',  ( -61.49999999999998579, 13.51041666598387003, 0.6339745962155628467 ) ) ;
#10962 = ORIENTED_EDGE ( 'NONE', *, *, #8078, .T. ) ;
#10963 = AXIS2_PLACEMENT_3D ( 'NONE', #5768, #9062, #1394 ) ;
#10964 = AXIS2_PLACEMENT_3D ( 'NONE', #10719, #9776, #9048 ) ;
#10965 = CARTESIAN_POINT ( 'NONE',  ( -61.99999999999998579, 14.01562499965860376, 2.498450539062049724 ) ) ;
#10966 = FILL_AREA_STYLE ('',( #10234 ) ) ;
#10967 = EDGE_LOOP ( 'NONE', ( #8193, #8284 ) ) ;
#10968 = EDGE_CURVE ( 'NONE', #10494, #7302, #8903, .T. ) ;
#10969 = CARTESIAN_POINT ( 'NONE',  ( 195.0000000000000000, 0.000000000000000000, 4.000000000000000000 ) ) ;
#10970 = VECTOR ( 'NONE', #2333, 1000.000000000000000 ) ;
#10971 = CARTESIAN_POINT ( 'NONE',  ( -61.13531646874998415, 12.66145833299193413, 1.000774730468978468 ) ) ;
#10972 = DIRECTION ( 'NONE',  ( 0.000000000000000000, 0.000000000000000000, -1.000000000000000000 ) ) ;
#10973 = EDGE_CURVE ( 'NONE', #8746, #7043, #10338, .T. ) ;
#10974 = VECTOR ( 'NONE', #9498, 1000.000000000000000 ) ;
#10975 = ORIENTED_EDGE ( 'NONE', *, *, #1748, .F. ) ;
#10976 = CARTESIAN_POINT ( 'NONE',  ( -120.0000000000000000, -15.00000000000001421, 0.000000000000000000 ) ) ;
#10977 = ORIENTED_EDGE ( 'NONE', *, *, #97, .F. ) ;
#10978 = CARTESIAN_POINT ( 'NONE',  ( -61.99999999999998579, 8.437500000000000000, 2.500000000000002665 ) ) ;
#10979 = VERTEX_POINT ( 'NONE', #337 ) ;
#10980 = CARTESIAN_POINT ( 'NONE',  ( -60.99999999999998579, 10.50000000000000000, 1.500000000000002220 ) ) ;
#10981 = CARTESIAN_POINT ( 'NONE',  ( -61.73205080756886076, 13.80133545031537068, 0.5000000000000014433 ) ) ;
#10982 = NEXT_ASSEMBLY_USAGE_OCCURRENCE ( 'NAUO1', ' ', ' ', #8478, #6528, $ ) ;
#10983 = NEXT_ASSEMBLY_USAGE_OCCURRENCE ( 'NAUO2', ' ', ' ', #8478, #10302, $ ) ;
#10984 = NEXT_ASSEMBLY_USAGE_OCCURRENCE ( 'NAUO3', ' ', ' ', #8478, #3118, $ ) ;
#10985 = NEXT_ASSEMBLY_USAGE_OCCURRENCE ( 'NAUO4', ' ', ' ', #8478, #1620, $ ) ;
#10986 = NEXT_ASSEMBLY_USAGE_OCCURRENCE ( 'NAUO5', ' ', ' ', #8478, #932, $ ) ;
#10987 = NEXT_ASSEMBLY_USAGE_OCCURRENCE ( 'NAUO6', ' ', ' ', #8478, #3253, $ ) ;
#10988 = NEXT_ASSEMBLY_USAGE_OCCURRENCE ( 'NAUO7', ' ', ' ', #8478, #5343, $ ) ;
#10989 = NEXT_ASSEMBLY_USAGE_OCCURRENCE ( 'NAUO8', ' ', ' ', #8478, #10791, $ ) ;
#10990 = NEXT_ASSEMBLY_USAGE_OCCURRENCE ( 'NAUO9', ' ', ' ', #8478, #10791, $ ) ;
#10991 = NEXT_ASSEMBLY_USAGE_OCCURRENCE ( 'NAUO10', ' ', ' ', #8478, #5895, $ ) ;
#10992 = NEXT_ASSEMBLY_USAGE_OCCURRENCE ( 'NAUO11', ' ', ' ', #8478, #5895, $ ) ;
#10993=COLOUR_RGB('Dark Blue',0.08,0.2,0.34);
#10994=FILL_AREA_STYLE_COLOUR('',#10993);
#10995=FILL_AREA_STYLE('',(#10994));
#10996=SURFACE_STYLE_FILL_AREA(#10995);
#10997=SURFACE_SIDE_STYLE('',(#10996));
#10998=SURFACE_STYLE_USAGE(.BOTH.,#10997);
#10999=PRESENTATION_STYLE_ASSIGNMENT((#10998));
#11000=COLOUR_RGB('Light Blue',0.38,0.62,0.78);
#11001=FILL_AREA_STYLE_COLOUR('',#11000);
#11002=FILL_AREA_STYLE('',(#11001));
#11003=SURFACE_STYLE_FILL_AREA(#11002);
#11004=SURFACE_SIDE_STYLE('',(#11003));
#11005=SURFACE_STYLE_USAGE(.BOTH.,#11004);
#11006=PRESENTATION_STYLE_ASSIGNMENT((#11005));
#11007=COLOUR_RGB('Sky Blue',0.24,0.69,0.87);
#11008=FILL_AREA_STYLE_COLOUR('',#11007);
#11009=FILL_AREA_STYLE('',(#11008));
#11010=SURFACE_STYLE_FILL_AREA(#11009);
#11011=SURFACE_SIDE_STYLE('',(#11010));
#11012=SURFACE_STYLE_USAGE(.BOTH.,#11011);
#11013=PRESENTATION_STYLE_ASSIGNMENT((#11012));
#11014=COLOUR_RGB('Grey',0.48,0.52,0.57);
#11015=FILL_AREA_STYLE_COLOUR('',#11014);
#11016=FILL_AREA_STYLE('',(#11015));
#11017=SURFACE_STYLE_FILL_AREA(#11016);
#11018=SURFACE_SIDE_STYLE('',(#11017));
#11019=SURFACE_STYLE_USAGE(.BOTH.,#11018);
#11020=PRESENTATION_STYLE_ASSIGNMENT((#11019));
#11021=COLOUR_RGB('Black',0.12,0.14,0.17);
#11022=FILL_AREA_STYLE_COLOUR('',#11021);
#11023=FILL_AREA_STYLE('',(#11022));
#11024=SURFACE_STYLE_FILL_AREA(#11023);
#11025=SURFACE_SIDE_STYLE('',(#11024));
#11026=SURFACE_STYLE_USAGE(.BOTH.,#11025);
#11027=PRESENTATION_STYLE_ASSIGNMENT((#11026));
#11028=COLOUR_RGB('Off White',0.89,0.88,0.83);
#11029=FILL_AREA_STYLE_COLOUR('',#11028);
#11030=FILL_AREA_STYLE('',(#11029));
#11031=SURFACE_STYLE_FILL_AREA(#11030);
#11032=SURFACE_SIDE_STYLE('',(#11031));
#11033=SURFACE_STYLE_USAGE(.BOTH.,#11032);
#11034=PRESENTATION_STYLE_ASSIGNMENT((#11033));
ENDSEC;
END-ISO-10303-21;
